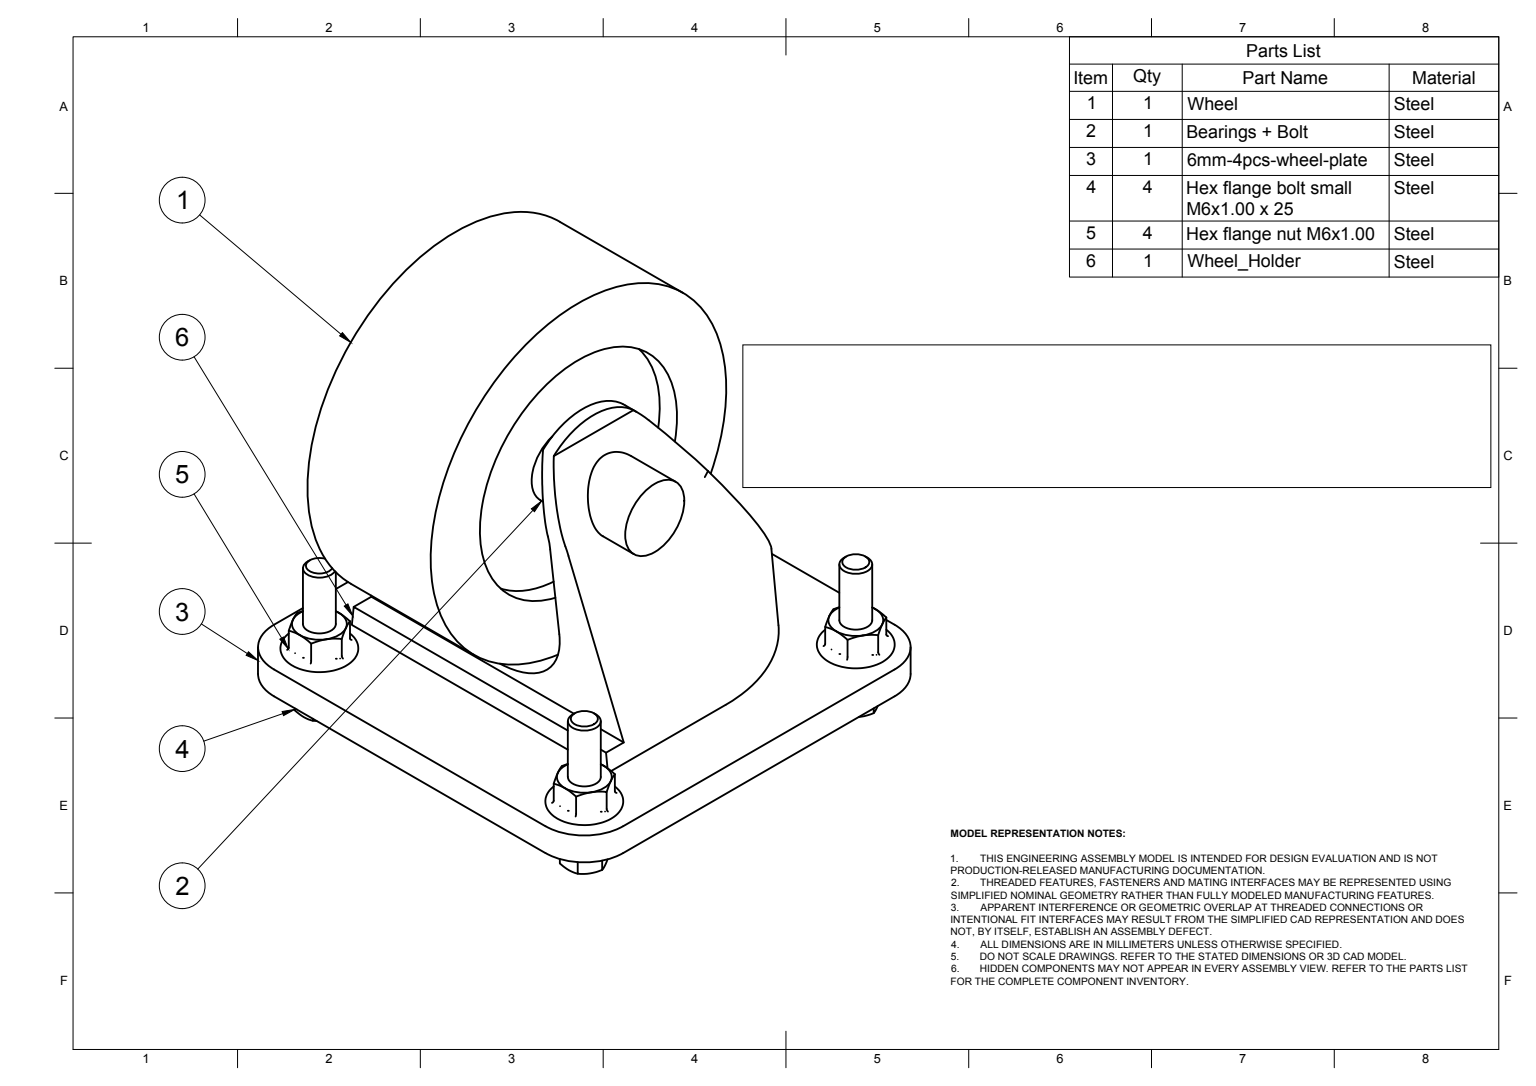
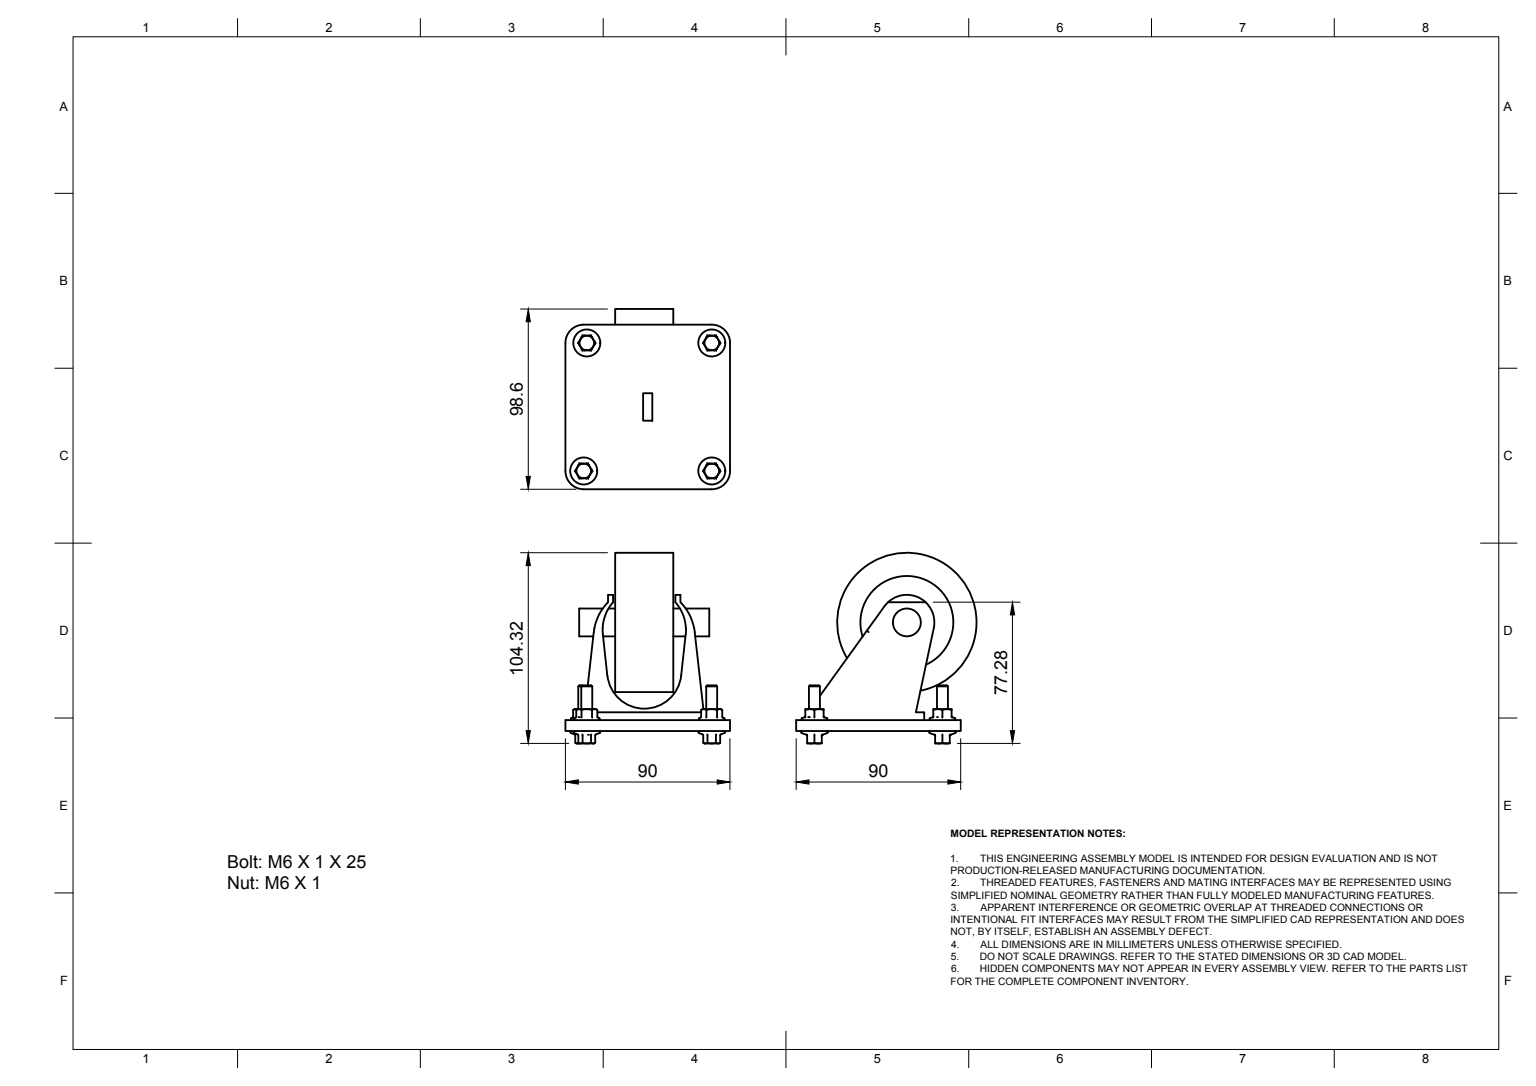
ISO-10303-21;
HEADER;
/* Generated by software containing ST-Developer
 * from STEP Tools, Inc. (www.steptools.com) 
 */

FILE_DESCRIPTION(
/* description */ ('Wheel Holder-Mirrored'),
/* implementation_level */ '2;1');

FILE_NAME(
/* name */ 'MAS-606',
/* time_stamp */ '2026-10-07T09:01:46-07:00',
/* author */ (''),
/* organization */ (''),
/* preprocessor_version */ 'ST-DEVELOPER v20.2',
/* originating_system */ 'Autodesk Translation Framework v15.15.0.0',
/* authorisation */ '');

FILE_SCHEMA (('AUTOMOTIVE_DESIGN { 1 0 10303 214 3 1 1 }'));
ENDSEC;

DATA;
#10=MECHANICAL_DESIGN_GEOMETRIC_PRESENTATION_REPRESENTATION('',(#198,#199,
#200,#201,#202,#203),#3832);
#11=ITEM_DEFINED_TRANSFORMATION($,$,#1857,#2036);
#12=ITEM_DEFINED_TRANSFORMATION($,$,#1874,#2037);
#13=ITEM_DEFINED_TRANSFORMATION($,$,#1880,#2038);
#14=ITEM_DEFINED_TRANSFORMATION($,$,#1915,#2039);
#15=ITEM_DEFINED_TRANSFORMATION($,$,#1951,#2040);
#16=ITEM_DEFINED_TRANSFORMATION($,$,#1915,#2041);
#17=ITEM_DEFINED_TRANSFORMATION($,$,#1915,#2042);
#18=ITEM_DEFINED_TRANSFORMATION($,$,#1915,#2043);
#19=ITEM_DEFINED_TRANSFORMATION($,$,#1951,#2044);
#20=ITEM_DEFINED_TRANSFORMATION($,$,#1951,#2045);
#21=ITEM_DEFINED_TRANSFORMATION($,$,#1951,#2046);
#22=ITEM_DEFINED_TRANSFORMATION($,$,#1986,#2047);
#23=(
REPRESENTATION_RELATIONSHIP($,$,#3863,#3862)
REPRESENTATION_RELATIONSHIP_WITH_TRANSFORMATION(#11)
SHAPE_REPRESENTATION_RELATIONSHIP()
);
#24=(
REPRESENTATION_RELATIONSHIP($,$,#3864,#3862)
REPRESENTATION_RELATIONSHIP_WITH_TRANSFORMATION(#12)
SHAPE_REPRESENTATION_RELATIONSHIP()
);
#25=(
REPRESENTATION_RELATIONSHIP($,$,#3865,#3862)
REPRESENTATION_RELATIONSHIP_WITH_TRANSFORMATION(#13)
SHAPE_REPRESENTATION_RELATIONSHIP()
);
#26=(
REPRESENTATION_RELATIONSHIP($,$,#3866,#3862)
REPRESENTATION_RELATIONSHIP_WITH_TRANSFORMATION(#14)
SHAPE_REPRESENTATION_RELATIONSHIP()
);
#27=(
REPRESENTATION_RELATIONSHIP($,$,#3867,#3862)
REPRESENTATION_RELATIONSHIP_WITH_TRANSFORMATION(#15)
SHAPE_REPRESENTATION_RELATIONSHIP()
);
#28=(
REPRESENTATION_RELATIONSHIP($,$,#3866,#3862)
REPRESENTATION_RELATIONSHIP_WITH_TRANSFORMATION(#16)
SHAPE_REPRESENTATION_RELATIONSHIP()
);
#29=(
REPRESENTATION_RELATIONSHIP($,$,#3866,#3862)
REPRESENTATION_RELATIONSHIP_WITH_TRANSFORMATION(#17)
SHAPE_REPRESENTATION_RELATIONSHIP()
);
#30=(
REPRESENTATION_RELATIONSHIP($,$,#3866,#3862)
REPRESENTATION_RELATIONSHIP_WITH_TRANSFORMATION(#18)
SHAPE_REPRESENTATION_RELATIONSHIP()
);
#31=(
REPRESENTATION_RELATIONSHIP($,$,#3867,#3862)
REPRESENTATION_RELATIONSHIP_WITH_TRANSFORMATION(#19)
SHAPE_REPRESENTATION_RELATIONSHIP()
);
#32=(
REPRESENTATION_RELATIONSHIP($,$,#3867,#3862)
REPRESENTATION_RELATIONSHIP_WITH_TRANSFORMATION(#20)
SHAPE_REPRESENTATION_RELATIONSHIP()
);
#33=(
REPRESENTATION_RELATIONSHIP($,$,#3867,#3862)
REPRESENTATION_RELATIONSHIP_WITH_TRANSFORMATION(#21)
SHAPE_REPRESENTATION_RELATIONSHIP()
);
#34=(
REPRESENTATION_RELATIONSHIP($,$,#3868,#3862)
REPRESENTATION_RELATIONSHIP_WITH_TRANSFORMATION(#22)
SHAPE_REPRESENTATION_RELATIONSHIP()
);
#35=CONTEXT_DEPENDENT_SHAPE_REPRESENTATION(#23,#3850);
#36=CONTEXT_DEPENDENT_SHAPE_REPRESENTATION(#24,#3851);
#37=CONTEXT_DEPENDENT_SHAPE_REPRESENTATION(#25,#3852);
#38=CONTEXT_DEPENDENT_SHAPE_REPRESENTATION(#26,#3853);
#39=CONTEXT_DEPENDENT_SHAPE_REPRESENTATION(#27,#3854);
#40=CONTEXT_DEPENDENT_SHAPE_REPRESENTATION(#28,#3855);
#41=CONTEXT_DEPENDENT_SHAPE_REPRESENTATION(#29,#3856);
#42=CONTEXT_DEPENDENT_SHAPE_REPRESENTATION(#30,#3857);
#43=CONTEXT_DEPENDENT_SHAPE_REPRESENTATION(#31,#3858);
#44=CONTEXT_DEPENDENT_SHAPE_REPRESENTATION(#32,#3859);
#45=CONTEXT_DEPENDENT_SHAPE_REPRESENTATION(#33,#3860);
#46=CONTEXT_DEPENDENT_SHAPE_REPRESENTATION(#34,#3861);
#47=NEXT_ASSEMBLY_USAGE_OCCURRENCE('Wheel:1','Wheel:1','Wheel:1',#3870,
#3871,'Wheel:1');
#48=NEXT_ASSEMBLY_USAGE_OCCURRENCE('Bearings + Bolt:1',
'Bearings + Bolt:1','Bearings + Bolt:1',#3870,#3872,'Bearings + Bolt:1');
#49=NEXT_ASSEMBLY_USAGE_OCCURRENCE('Wheel_Plate:1','Wheel_Plate:1',
'Wheel_Plate:1',#3870,#3873,'Wheel_Plate:1');
#50=NEXT_ASSEMBLY_USAGE_OCCURRENCE(
'Hex flange bolt small M6x1.00 x 25:1',
'Hex flange bolt small M6x1.00 x 25:1',
'Hex flange bolt small M6x1.00 x 25:1',#3870,#3874,
'Hex flange bolt small M6x1.00 x 25:1');
#51=NEXT_ASSEMBLY_USAGE_OCCURRENCE('Hex flange nut M6x1.00:1',
'Hex flange nut M6x1.00:1','Hex flange nut M6x1.00:1',#3870,#3875,
'Hex flange nut M6x1.00:1');
#52=NEXT_ASSEMBLY_USAGE_OCCURRENCE(
'Hex flange bolt small M6x1.00 x 25:2',
'Hex flange bolt small M6x1.00 x 25:2',
'Hex flange bolt small M6x1.00 x 25:2',#3870,#3874,
'Hex flange bolt small M6x1.00 x 25:2');
#53=NEXT_ASSEMBLY_USAGE_OCCURRENCE(
'Hex flange bolt small M6x1.00 x 25:3',
'Hex flange bolt small M6x1.00 x 25:3',
'Hex flange bolt small M6x1.00 x 25:3',#3870,#3874,
'Hex flange bolt small M6x1.00 x 25:3');
#54=NEXT_ASSEMBLY_USAGE_OCCURRENCE(
'Hex flange bolt small M6x1.00 x 25:4',
'Hex flange bolt small M6x1.00 x 25:4',
'Hex flange bolt small M6x1.00 x 25:4',#3870,#3874,
'Hex flange bolt small M6x1.00 x 25:4');
#55=NEXT_ASSEMBLY_USAGE_OCCURRENCE('Hex flange nut M6x1.00:2',
'Hex flange nut M6x1.00:2','Hex flange nut M6x1.00:2',#3870,#3875,
'Hex flange nut M6x1.00:2');
#56=NEXT_ASSEMBLY_USAGE_OCCURRENCE('Hex flange nut M6x1.00:3',
'Hex flange nut M6x1.00:3','Hex flange nut M6x1.00:3',#3870,#3875,
'Hex flange nut M6x1.00:3');
#57=NEXT_ASSEMBLY_USAGE_OCCURRENCE('Hex flange nut M6x1.00:4',
'Hex flange nut M6x1.00:4','Hex flange nut M6x1.00:4',#3870,#3875,
'Hex flange nut M6x1.00:4');
#58=NEXT_ASSEMBLY_USAGE_OCCURRENCE('Wheel_Holder:1','Wheel_Holder:1',
'Wheel_Holder:1',#3870,#3876,'Wheel_Holder:1');
#59=ELLIPSE('',#1988,0.00766814592499653,0.00762);
#60=ELLIPSE('',#1989,0.0076644002839305,0.00762);
#61=ELLIPSE('',#1993,0.0342294027026876,0.0277785949688766);
#62=ELLIPSE('',#1994,0.028399185304996,0.0277785949688766);
#63=ELLIPSE('',#2002,0.0232756976080203,0.0227670677706907);
#64=ELLIPSE('',#2003,0.0280540873991463,0.0227670677706907);
#65=ELLIPSE('',#2005,0.0232756976080203,0.0227670677706907);
#66=ELLIPSE('',#2006,0.0280540873991463,0.0227670677706907);
#67=ELLIPSE('',#2009,0.0207739608876574,0.02032);
#68=ELLIPSE('',#2010,0.0250387560529214,0.02032);
#69=ELLIPSE('',#2012,0.0076644002839305,0.00762);
#70=ELLIPSE('',#2016,0.0283991853049961,0.0277785949688767);
#71=ELLIPSE('',#2021,0.0570304735096183,0.0331133532215094);
#72=ELLIPSE('',#2022,0.0342294027026876,0.0277785949688767);
#73=ELLIPSE('',#2023,0.0570304735096183,0.0331133532215094);
#74=ELLIPSE('',#2025,0.0333225754026887,0.0331133532215094);
#75=ELLIPSE('',#2026,0.0333225754026887,0.0331133532215094);
#76=ELLIPSE('',#2028,0.00766814592499653,0.00762);
#77=ELLIPSE('',#2034,0.295962272640151,0.0331133532215094);
#78=(
BOUNDED_SURFACE()
B_SPLINE_SURFACE(3,2,((#2888,#2889,#2890),(#2891,#2892,#2893),(#2894,#2895,
#2896),(#2897,#2898,#2899),(#2900,#2901,#2902)),.UNSPECIFIED.,.F.,.F.,.F.)
B_SPLINE_SURFACE_WITH_KNOTS((4,1,4),(3,3),(0.0199905421078539,0.0227092821601536,
0.0254280222134474),(0.,1.00056005679341),.UNSPECIFIED.)
GEOMETRIC_REPRESENTATION_ITEM()
RATIONAL_B_SPLINE_SURFACE(((1.,0.802854637372621,1.00022082519925),(1.,
0.81108958019377,1.00021160112791),(1.,0.82690910145913,1.00019388146721),
(1.,0.811291833393597,1.00021137458136),(1.,0.802795753782992,1.00022089115557)))
REPRESENTATION_ITEM('')
SURFACE()
);
#79=(
BOUNDED_SURFACE()
B_SPLINE_SURFACE(3,2,((#2927,#2928,#2929),(#2930,#2931,#2932),(#2933,#2934,
#2935),(#2936,#2937,#2938),(#2939,#2940,#2941)),.UNSPECIFIED.,.F.,.F.,.F.)
B_SPLINE_SURFACE_WITH_KNOTS((4,1,4),(3,3),(0.0199863987269074,0.0227063701116868,
0.0254263415355543),(0.,1.00056355085534),.UNSPECIFIED.)
GEOMETRIC_REPRESENTATION_ITEM()
RATIONAL_B_SPLINE_SURFACE(((1.,0.802841957060873,1.00022221716746),(1.,
0.811080854660757,1.00021293109189),(1.,0.826916200792063,1.00019508304617),
(1.,0.811283787847418,1.00021270236556),(1.,0.802782519169589,1.00022228416001)))
REPRESENTATION_ITEM('')
SURFACE()
);
#80=(
BOUNDED_SURFACE()
B_SPLINE_SURFACE(3,2,((#2954,#2955,#2956),(#2957,#2958,#2959),(#2960,#2961,
#2962),(#2963,#2964,#2965),(#2966,#2967,#2968)),.UNSPECIFIED.,.F.,.F.,.F.)
B_SPLINE_SURFACE_WITH_KNOTS((4,1,4),(3,3),(0.0199905421079487,0.0227092821601536,
0.0254280222133526),(0.,1.00056005680003),.UNSPECIFIED.)
GEOMETRIC_REPRESENTATION_ITEM()
RATIONAL_B_SPLINE_SURFACE(((1.,0.802854637372034,1.00022082520187),(1.,
0.811089580193672,1.00021160113042),(1.,0.826909101456828,1.00019388146951),
(1.,0.81129183339351,1.00021137458386),(1.,0.802795753782428,1.00022089115817)))
REPRESENTATION_ITEM('')
SURFACE()
);
#81=(
BOUNDED_SURFACE()
B_SPLINE_SURFACE(3,2,((#2981,#2982,#2983),(#2984,#2985,#2986),(#2987,#2988,
#2989),(#2990,#2991,#2992),(#2993,#2994,#2995)),.UNSPECIFIED.,.F.,.F.,.F.)
B_SPLINE_SURFACE_WITH_KNOTS((4,1,4),(3,3),(0.0199905421080522,0.0227092821601536,
0.0254280222132491),(0.,1.00056005679973),.UNSPECIFIED.)
GEOMETRIC_REPRESENTATION_ITEM()
RATIONAL_B_SPLINE_SURFACE(((1.,0.802854637372995,1.00022082520174),(1.,
0.811089580194489,1.00021160113031),(1.,0.826909101456198,1.0001938814694),
(1.,0.811291833394166,1.00021137458374),(1.,0.802795753783457,1.00022089115806)))
REPRESENTATION_ITEM('')
SURFACE()
);
#82=(
BOUNDED_SURFACE()
B_SPLINE_SURFACE(3,2,((#3008,#3009,#3010),(#3011,#3012,#3013),(#3014,#3015,
#3016),(#3017,#3018,#3019),(#3020,#3021,#3022)),.UNSPECIFIED.,.F.,.F.,.F.)
B_SPLINE_SURFACE_WITH_KNOTS((4,1,4),(3,3),(0.019994704332767,0.022712204724463,
0.0254297050789377),(0.,1.00055654499458),.UNSPECIFIED.)
GEOMETRIC_REPRESENTATION_ITEM()
RATIONAL_B_SPLINE_SURFACE(((1.,0.802867397371381,1.00021942632651),(1.,
0.811098353635701,1.00021026453151),(1.,0.826901960236561,1.00019267369521),
(1.,0.811299927383003,1.00021004016178),(1.,0.802809067580306,1.00021949125283)))
REPRESENTATION_ITEM('')
SURFACE()
);
#83=(
BOUNDED_SURFACE()
B_SPLINE_SURFACE(3,2,((#3035,#3036,#3037),(#3038,#3039,#3040),(#3041,#3042,
#3043),(#3044,#3045,#3046),(#3047,#3048,#3049)),.UNSPECIFIED.,.F.,.F.,.F.)
B_SPLINE_SURFACE_WITH_KNOTS((4,1,4),(3,3),(0.0199905421078943,0.0227092821601536,
0.025428022213407),(0.,1.00056005680679),.UNSPECIFIED.)
GEOMETRIC_REPRESENTATION_ITEM()
RATIONAL_B_SPLINE_SURFACE(((1.,0.802854637370352,1.00022082520454),(1.,
0.811089580191479,1.00021160113298),(1.,0.826909101456581,1.00019388147184),
(1.,0.811291833391307,1.00021137458641),(1.,0.802795753780734,1.00022089116085)))
REPRESENTATION_ITEM('')
SURFACE()
);
#84=(
BOUNDED_SURFACE()
B_SPLINE_SURFACE(3,2,((#3298,#3299,#3300),(#3301,#3302,#3303),(#3304,#3305,
#3306),(#3307,#3308,#3309),(#3310,#3311,#3312)),.UNSPECIFIED.,.F.,.F.,.F.)
B_SPLINE_SURFACE_WITH_KNOTS((4,1,4),(3,3),(0.0246620904109836,0.0279939304185144,
0.0313257704892837),(0.,1.00067047018092),.UNSPECIFIED.)
GEOMETRIC_REPRESENTATION_ITEM()
RATIONAL_B_SPLINE_SURFACE(((1.,0.802865969663045,1.00026434497797),(1.,
0.81108910405605,1.00025331824517),(1.,0.82686917993846,1.0002321581045),
(1.,0.81129221048254,1.00025304589156),(1.,0.802807804958138,1.00026442297338)))
REPRESENTATION_ITEM('')
SURFACE()
);
#85=(
BOUNDED_SURFACE()
B_SPLINE_SURFACE(3,2,((#3337,#3338,#3339),(#3340,#3341,#3342),(#3343,#3344,
#3345),(#3346,#3347,#3348),(#3349,#3350,#3351)),.UNSPECIFIED.,.F.,.F.,.F.)
B_SPLINE_SURFACE_WITH_KNOTS((4,1,4),(3,3),(0.024738817097226,0.0280688166766824,
0.0313988162601249),(0.,1.00066549850917),.UNSPECIFIED.)
GEOMETRIC_REPRESENTATION_ITEM()
RATIONAL_B_SPLINE_SURFACE(((1.,0.802880827397706,1.00026236503099),(1.,
0.811099228845429,1.00025142636317),(1.,0.82686120340028,1.00023044722203),
(1.,0.811301685281914,1.00025115689426),(1.,0.80282325859447,1.0002624416549)))
REPRESENTATION_ITEM('')
SURFACE()
);
#86=(
BOUNDED_SURFACE()
B_SPLINE_SURFACE(3,2,((#3364,#3365,#3366),(#3367,#3368,#3369),(#3370,#3371,
#3372),(#3373,#3374,#3375),(#3376,#3377,#3378)),.UNSPECIFIED.,.F.,.F.,.F.)
B_SPLINE_SURFACE_WITH_KNOTS((4,1,4),(3,3),(0.024738817096804,0.0280688166766824,
0.0313988162605461),(0.,1.00066549851789),.UNSPECIFIED.)
GEOMETRIC_REPRESENTATION_ITEM()
RATIONAL_B_SPLINE_SURFACE(((1.,0.802880827392752,1.00026236503443),(1.,
0.811099228842278,1.00025142636647),(1.,0.826861203399938,1.00023044722505),
(1.,0.811301685279444,1.00025115689755),(1.,0.802823258589269,1.00026244165835)))
REPRESENTATION_ITEM('')
SURFACE()
);
#87=(
BOUNDED_SURFACE()
B_SPLINE_SURFACE(3,2,((#3391,#3392,#3393),(#3394,#3395,#3396),(#3397,#3398,
#3399),(#3400,#3401,#3402),(#3403,#3404,#3405)),.UNSPECIFIED.,.F.,.F.,.F.)
B_SPLINE_SURFACE_WITH_KNOTS((4,1,4),(3,3),(0.0247388170968889,0.0280688166766824,
0.0313988162604618),(0.,1.00066549851781),.UNSPECIFIED.)
GEOMETRIC_REPRESENTATION_ITEM()
RATIONAL_B_SPLINE_SURFACE(((1.,0.802880827393329,1.00026236503441),(1.,
0.811099228842959,1.00025142636643),(1.,0.82686120340021,1.00023044722503),
(1.,0.811301685278279,1.00025115689751),(1.,0.802823258590303,1.0002624416583)))
REPRESENTATION_ITEM('')
SURFACE()
);
#88=(
BOUNDED_SURFACE()
B_SPLINE_SURFACE(3,2,((#3418,#3419,#3420),(#3421,#3422,#3423),(#3424,#3425,
#3426),(#3427,#3428,#3429),(#3430,#3431,#3432)),.UNSPECIFIED.,.F.,.F.,.F.)
B_SPLINE_SURFACE_WITH_KNOTS((4,1,4),(3,3),(0.0247388170974279,0.0280688166766824,
0.031398816259923),(0.,1.00066549852508),.UNSPECIFIED.)
GEOMETRIC_REPRESENTATION_ITEM()
RATIONAL_B_SPLINE_SURFACE(((1.,0.802880827396021,1.00026236503726),(1.,
0.811099228843575,1.00025142636918),(1.,0.826861203396443,1.00023044722754),
(1.,0.811301685279931,1.00025115690027),(1.,0.80282325859286,1.00026244166118)))
REPRESENTATION_ITEM('')
SURFACE()
);
#89=(
BOUNDED_SURFACE()
B_SPLINE_SURFACE(3,2,((#3445,#3446,#3447),(#3448,#3449,#3450),(#3451,#3452,
#3453),(#3454,#3455,#3456),(#3457,#3458,#3459)),.UNSPECIFIED.,.F.,.F.,.F.)
B_SPLINE_SURFACE_WITH_KNOTS((4,1,4),(3,3),(0.0246749646102296,0.0280029916911416,
0.031331018716321),(0.,1.00065966906838),.UNSPECIFIED.)
GEOMETRIC_REPRESENTATION_ITEM()
RATIONAL_B_SPLINE_SURFACE(((1.,0.802898366215555,1.00026004370227),(1.,
0.811111461933951,1.00024920785186),(1.,0.826851645151749,1.00022844122787),
(1.,0.811312849119053,1.00024894215407),(1.,0.802841584394648,1.00026011861669)))
REPRESENTATION_ITEM('')
SURFACE()
);
#90=TOROIDAL_SURFACE('',#1935,0.0068,0.000567100162269167);
#91=TOROIDAL_SURFACE('',#1948,0.00325,0.00025);
#92=TOROIDAL_SURFACE('',#1982,0.00653289983773083,0.000567100162269171);
#93=CONICAL_SURFACE('',#1922,0.004,1.0471975511966);
#94=CONICAL_SURFACE('',#1924,0.004,1.0471975511966);
#95=CONICAL_SURFACE('',#1926,0.004,1.0471975511966);
#96=CONICAL_SURFACE('',#1928,0.004,1.0471975511966);
#97=CONICAL_SURFACE('',#1930,0.004,1.0471975511966);
#98=CONICAL_SURFACE('',#1932,0.004,1.0471975511966);
#99=CONICAL_SURFACE('',#1940,1.,1.22173047639603);
#100=CONICAL_SURFACE('',#1950,0.002458734125,0.78539816339745);
#101=CONICAL_SURFACE('',#1973,0.005,1.0471975511966);
#102=CONICAL_SURFACE('',#1974,0.005,1.0471975511966);
#103=CONICAL_SURFACE('',#1975,0.005,1.0471975511966);
#104=CONICAL_SURFACE('',#1976,0.005,1.0471975511966);
#105=CONICAL_SURFACE('',#1977,0.005,1.0471975511966);
#106=CONICAL_SURFACE('',#1978,0.005,1.0471975511966);
#107=CONICAL_SURFACE('',#1979,0.00672685951651014,1.22173047639603);
#108=CONICAL_SURFACE('',#1984,0.003,0.785398163397448);
#109=CONICAL_SURFACE('',#1985,0.0024585,0.785398163397448);
#110=(
BOUNDED_CURVE()
B_SPLINE_CURVE(2,(#2688,#2689,#2690),.UNSPECIFIED.,.F.,.F.)
B_SPLINE_CURVE_WITH_KNOTS((3,3),(0.899640233852609,1.41204223156836),
 .UNSPECIFIED.)
CURVE()
GEOMETRIC_REPRESENTATION_ITEM()
RATIONAL_B_SPLINE_CURVE((2.04103265936813,2.19890708499154,2.19890708499154))
REPRESENTATION_ITEM('')
);
#111=(
BOUNDED_CURVE()
B_SPLINE_CURVE(2,(#2691,#2692,#2693),.UNSPECIFIED.,.F.,.F.)
B_SPLINE_CURVE_WITH_KNOTS((3,3),(1.41204223156836,1.92444422930209),
 .UNSPECIFIED.)
CURVE()
GEOMETRIC_REPRESENTATION_ITEM()
RATIONAL_B_SPLINE_CURVE((2.19890708499154,2.19890708499154,2.04103265935705))
REPRESENTATION_ITEM('')
);
#112=(
BOUNDED_CURVE()
B_SPLINE_CURVE(2,(#2715,#2716,#2717),.UNSPECIFIED.,.F.,.F.)
B_SPLINE_CURVE_WITH_KNOTS((3,3),(0.899640233852608,1.41204223156835),
 .UNSPECIFIED.)
CURVE()
GEOMETRIC_REPRESENTATION_ITEM()
RATIONAL_B_SPLINE_CURVE((2.04103265936813,2.19890708499154,2.19890708499154))
REPRESENTATION_ITEM('')
);
#113=(
BOUNDED_CURVE()
B_SPLINE_CURVE(2,(#2718,#2719,#2720),.UNSPECIFIED.,.F.,.F.)
B_SPLINE_CURVE_WITH_KNOTS((3,3),(1.41204223156835,1.9244442293021),
 .UNSPECIFIED.)
CURVE()
GEOMETRIC_REPRESENTATION_ITEM()
RATIONAL_B_SPLINE_CURVE((2.19890708499154,2.19890708499154,2.04103265935704))
REPRESENTATION_ITEM('')
);
#114=(
BOUNDED_CURVE()
B_SPLINE_CURVE(2,(#2742,#2743,#2744),.UNSPECIFIED.,.F.,.F.)
B_SPLINE_CURVE_WITH_KNOTS((3,3),(-1.41204232189231,-0.899640300628516),
 .UNSPECIFIED.)
CURVE()
GEOMETRIC_REPRESENTATION_ITEM()
RATIONAL_B_SPLINE_CURVE((2.19890717995419,2.19890717995419,2.04103274751277))
REPRESENTATION_ITEM('')
);
#115=(
BOUNDED_CURVE()
B_SPLINE_CURVE(2,(#2745,#2746,#2747),.UNSPECIFIED.,.F.,.F.)
B_SPLINE_CURVE_WITH_KNOTS((3,3),(-1.9244443431741,-1.41204232189231),
 .UNSPECIFIED.)
CURVE()
GEOMETRIC_REPRESENTATION_ITEM()
RATIONAL_B_SPLINE_CURVE((2.04103274750169,2.19890717995419,2.19890717995419))
REPRESENTATION_ITEM('')
);
#116=(
BOUNDED_CURVE()
B_SPLINE_CURVE(2,(#2769,#2770,#2771),.UNSPECIFIED.,.F.,.F.)
B_SPLINE_CURVE_WITH_KNOTS((3,3),(0.899640233852631,1.41204223156839),
 .UNSPECIFIED.)
CURVE()
GEOMETRIC_REPRESENTATION_ITEM()
RATIONAL_B_SPLINE_CURVE((2.04103265936816,2.19890708499158,2.19890708499158))
REPRESENTATION_ITEM('')
);
#117=(
BOUNDED_CURVE()
B_SPLINE_CURVE(2,(#2772,#2773,#2774),.UNSPECIFIED.,.F.,.F.)
B_SPLINE_CURVE_WITH_KNOTS((3,3),(1.41204223156839,1.92444422930213),
 .UNSPECIFIED.)
CURVE()
GEOMETRIC_REPRESENTATION_ITEM()
RATIONAL_B_SPLINE_CURVE((2.19890708499158,2.19890708499158,2.04103265935708))
REPRESENTATION_ITEM('')
);
#118=(
BOUNDED_CURVE()
B_SPLINE_CURVE(2,(#2796,#2797,#2798),.UNSPECIFIED.,.F.,.F.)
B_SPLINE_CURVE_WITH_KNOTS((3,3),(0.899640233852618,1.41204223156836),
 .UNSPECIFIED.)
CURVE()
GEOMETRIC_REPRESENTATION_ITEM()
RATIONAL_B_SPLINE_CURVE((2.04103265936815,2.19890708499156,2.19890708499156))
REPRESENTATION_ITEM('')
);
#119=(
BOUNDED_CURVE()
B_SPLINE_CURVE(2,(#2799,#2800,#2801),.UNSPECIFIED.,.F.,.F.)
B_SPLINE_CURVE_WITH_KNOTS((3,3),(1.41204223156836,1.92444422930211),
 .UNSPECIFIED.)
CURVE()
GEOMETRIC_REPRESENTATION_ITEM()
RATIONAL_B_SPLINE_CURVE((2.19890708499156,2.19890708499156,2.04103265935706))
REPRESENTATION_ITEM('')
);
#120=(
BOUNDED_CURVE()
B_SPLINE_CURVE(2,(#2820,#2821,#2822),.UNSPECIFIED.,.F.,.F.)
B_SPLINE_CURVE_WITH_KNOTS((3,3),(0.899640166945249,1.4120421410666),
 .UNSPECIFIED.)
CURVE()
GEOMETRIC_REPRESENTATION_ITEM()
RATIONAL_B_SPLINE_CURVE((2.04103257104998,2.19890698984196,2.19890698984195))
REPRESENTATION_ITEM('')
);
#121=(
BOUNDED_CURVE()
B_SPLINE_CURVE(2,(#2823,#2824,#2825),.UNSPECIFIED.,.F.,.F.)
B_SPLINE_CURVE_WITH_KNOTS((3,3),(1.4120421410666,1.92444411520593),
 .UNSPECIFIED.)
CURVE()
GEOMETRIC_REPRESENTATION_ITEM()
RATIONAL_B_SPLINE_CURVE((2.19890698984195,2.19890698984195,2.04103257103889))
REPRESENTATION_ITEM('')
);
#122=(
BOUNDED_CURVE()
B_SPLINE_CURVE(2,(#3088,#3089,#3090),.UNSPECIFIED.,.F.,.F.)
B_SPLINE_CURVE_WITH_KNOTS((3,3),(0.868406024324111,1.41937586994552),
 .UNSPECIFIED.)
CURVE()
GEOMETRIC_REPRESENTATION_ITEM()
RATIONAL_B_SPLINE_CURVE((1.77300211797113,1.91014430907105,1.91014430907105))
REPRESENTATION_ITEM('')
);
#123=(
BOUNDED_CURVE()
B_SPLINE_CURVE(2,(#3091,#3092,#3093),.UNSPECIFIED.,.F.,.F.)
B_SPLINE_CURVE_WITH_KNOTS((3,3),(1.41937586994552,1.97034571556692),
 .UNSPECIFIED.)
CURVE()
GEOMETRIC_REPRESENTATION_ITEM()
RATIONAL_B_SPLINE_CURVE((1.91014430907105,1.91014430907105,1.77300211797113))
REPRESENTATION_ITEM('')
);
#124=(
BOUNDED_CURVE()
B_SPLINE_CURVE(2,(#3115,#3116,#3117),.UNSPECIFIED.,.F.,.F.)
B_SPLINE_CURVE_WITH_KNOTS((3,3),(0.868406111432395,1.41937598717132),
 .UNSPECIFIED.)
CURVE()
GEOMETRIC_REPRESENTATION_ITEM()
RATIONAL_B_SPLINE_CURVE((1.7730022081019,1.91014440617345,1.91014440617345))
REPRESENTATION_ITEM('')
);
#125=(
BOUNDED_CURVE()
B_SPLINE_CURVE(2,(#3118,#3119,#3120),.UNSPECIFIED.,.F.,.F.)
B_SPLINE_CURVE_WITH_KNOTS((3,3),(1.41937598717132,1.97034586291024),
 .UNSPECIFIED.)
CURVE()
GEOMETRIC_REPRESENTATION_ITEM()
RATIONAL_B_SPLINE_CURVE((1.91014440617345,1.91014440617345,1.7730022081019))
REPRESENTATION_ITEM('')
);
#126=(
BOUNDED_CURVE()
B_SPLINE_CURVE(2,(#3142,#3143,#3144),.UNSPECIFIED.,.F.,.F.)
B_SPLINE_CURVE_WITH_KNOTS((3,3),(0.868406111432417,1.41937598717135),
 .UNSPECIFIED.)
CURVE()
GEOMETRIC_REPRESENTATION_ITEM()
RATIONAL_B_SPLINE_CURVE((1.77300220810192,1.91014440617348,1.91014440617348))
REPRESENTATION_ITEM('')
);
#127=(
BOUNDED_CURVE()
B_SPLINE_CURVE(2,(#3145,#3146,#3147),.UNSPECIFIED.,.F.,.F.)
B_SPLINE_CURVE_WITH_KNOTS((3,3),(1.41937598717135,1.97034586291028),
 .UNSPECIFIED.)
CURVE()
GEOMETRIC_REPRESENTATION_ITEM()
RATIONAL_B_SPLINE_CURVE((1.91014440617348,1.91014440617348,1.77300220810192))
REPRESENTATION_ITEM('')
);
#128=(
BOUNDED_CURVE()
B_SPLINE_CURVE(2,(#3169,#3170,#3171),.UNSPECIFIED.,.F.,.F.)
B_SPLINE_CURVE_WITH_KNOTS((3,3),(-1.41937608879025,-0.868406186943507),
 .UNSPECIFIED.)
CURVE()
GEOMETRIC_REPRESENTATION_ITEM()
RATIONAL_B_SPLINE_CURVE((1.91014449034812,1.91014449034812,1.7730022862331))
REPRESENTATION_ITEM('')
);
#129=(
BOUNDED_CURVE()
B_SPLINE_CURVE(2,(#3172,#3173,#3174),.UNSPECIFIED.,.F.,.F.)
B_SPLINE_CURVE_WITH_KNOTS((3,3),(-1.97034599063699,-1.41937608879025),
 .UNSPECIFIED.)
CURVE()
GEOMETRIC_REPRESENTATION_ITEM()
RATIONAL_B_SPLINE_CURVE((1.7730022862331,1.91014449034812,1.91014449034812))
REPRESENTATION_ITEM('')
);
#130=(
BOUNDED_CURVE()
B_SPLINE_CURVE(2,(#3196,#3197,#3198),.UNSPECIFIED.,.F.,.F.)
B_SPLINE_CURVE_WITH_KNOTS((3,3),(0.868406111432395,1.41937598717132),
 .UNSPECIFIED.)
CURVE()
GEOMETRIC_REPRESENTATION_ITEM()
RATIONAL_B_SPLINE_CURVE((1.7730022081019,1.91014440617345,1.91014440617345))
REPRESENTATION_ITEM('')
);
#131=(
BOUNDED_CURVE()
B_SPLINE_CURVE(2,(#3199,#3200,#3201),.UNSPECIFIED.,.F.,.F.)
B_SPLINE_CURVE_WITH_KNOTS((3,3),(1.41937598717132,1.97034586291024),
 .UNSPECIFIED.)
CURVE()
GEOMETRIC_REPRESENTATION_ITEM()
RATIONAL_B_SPLINE_CURVE((1.91014440617345,1.91014440617345,1.7730022081019))
REPRESENTATION_ITEM('')
);
#132=(
BOUNDED_CURVE()
B_SPLINE_CURVE(2,(#3220,#3221,#3222),.UNSPECIFIED.,.F.,.F.)
B_SPLINE_CURVE_WITH_KNOTS((3,3),(0.868406111432386,1.41937598717131),
 .UNSPECIFIED.)
CURVE()
GEOMETRIC_REPRESENTATION_ITEM()
RATIONAL_B_SPLINE_CURVE((1.77300220810189,1.91014440617345,1.91014440617345))
REPRESENTATION_ITEM('')
);
#133=(
BOUNDED_CURVE()
B_SPLINE_CURVE(2,(#3223,#3224,#3225),.UNSPECIFIED.,.F.,.F.)
B_SPLINE_CURVE_WITH_KNOTS((3,3),(1.41937598717131,1.97034586291023),
 .UNSPECIFIED.)
CURVE()
GEOMETRIC_REPRESENTATION_ITEM()
RATIONAL_B_SPLINE_CURVE((1.91014440617345,1.91014440617345,1.77300220810189))
REPRESENTATION_ITEM('')
);
#134=B_SPLINE_CURVE_WITH_KNOTS('',3,(#2669,#2670,#2671,#2672,#2673,#2674,
#2675,#2676,#2677,#2678,#2679,#2680,#2681,#2682,#2683,#2684),
 .UNSPECIFIED.,.F.,.F.,(4,3,3,3,3,4),(0.,0.00115933810312788,0.0023008628112466,
0.00231867620625576,0.00347801430938363,0.00463735241251151),
 .UNSPECIFIED.);
#135=B_SPLINE_CURVE_WITH_KNOTS('',3,(#2696,#2697,#2698,#2699,#2700,#2701,
#2702,#2703,#2704,#2705,#2706,#2707,#2708,#2709,#2710,#2711),
 .UNSPECIFIED.,.F.,.F.,(4,3,3,3,3,4),(1.55309542619116E-19,0.00115933810312788,
0.0023008628112466,0.00231867620625576,0.00347801430938364,0.00463735241251152),
 .UNSPECIFIED.);
#136=B_SPLINE_CURVE_WITH_KNOTS('',3,(#2723,#2724,#2725,#2726,#2727,#2728,
#2729,#2730,#2731,#2732,#2733,#2734,#2735,#2736,#2737,#2738),
 .UNSPECIFIED.,.F.,.F.,(4,3,3,3,3,4),(0.,0.00115932447661246,0.00230074676248248,
0.00231864895322491,0.00347797342983737,0.00463729790644982),
 .UNSPECIFIED.);
#137=B_SPLINE_CURVE_WITH_KNOTS('',3,(#2750,#2751,#2752,#2753,#2754,#2755,
#2756,#2757,#2758,#2759,#2760,#2761,#2762,#2763,#2764,#2765),
 .UNSPECIFIED.,.F.,.F.,(4,3,3,3,3,4),(0.,0.00115933810312788,0.0023008628112466,
0.00231867620625576,0.00347801430938363,0.00463735241251151),
 .UNSPECIFIED.);
#138=B_SPLINE_CURVE_WITH_KNOTS('',3,(#2777,#2778,#2779,#2780,#2781,#2782,
#2783,#2784,#2785,#2786,#2787,#2788,#2789,#2790,#2791,#2792),
 .UNSPECIFIED.,.F.,.F.,(4,3,3,3,3,4),(3.24894099173316E-19,0.00115933810312788,
0.0023008628112466,0.00231867620625576,0.00347801430938364,0.00463735241251152),
 .UNSPECIFIED.);
#139=B_SPLINE_CURVE_WITH_KNOTS('',3,(#2803,#2804,#2805,#2806,#2807,#2808,
#2809,#2810,#2811,#2812,#2813,#2814,#2815,#2816,#2817,#2818),
 .UNSPECIFIED.,.F.,.F.,(4,3,3,3,3,4),(0.,0.00115935174734299,0.00230097898664969,
0.00231870349468598,0.00347805524202897,0.00463740698937197),
 .UNSPECIFIED.);
#140=B_SPLINE_CURVE_WITH_KNOTS('',3,(#2851,#2852,#2853,#2854,#2855),
 .UNSPECIFIED.,.F.,.F.,(4,1,4),(0.,0.00248123639135078,0.00496246810726153),
 .UNSPECIFIED.);
#141=B_SPLINE_CURVE_WITH_KNOTS('',3,(#2857,#2858,#2859,#2860,#2861),
 .UNSPECIFIED.,.F.,.F.,(4,1,4),(0.,0.00248125883902994,0.00496251282372695),
 .UNSPECIFIED.);
#142=B_SPLINE_CURVE_WITH_KNOTS('',3,(#2863,#2864,#2865,#2866,#2867),
 .UNSPECIFIED.,.F.,.F.,(4,1,4),(0.,0.00248123639135078,0.00496246796815217),
 .UNSPECIFIED.);
#143=B_SPLINE_CURVE_WITH_KNOTS('',3,(#2869,#2870,#2871,#2872,#2873),
 .UNSPECIFIED.,.F.,.F.,(4,1,4),(0.,0.00248123639135079,0.00496246818443855),
 .UNSPECIFIED.);
#144=B_SPLINE_CURVE_WITH_KNOTS('',3,(#2875,#2876,#2877,#2878,#2879),
 .UNSPECIFIED.,.F.,.F.,(4,1,4),(0.,0.00248121396259867,0.00496242332668108),
 .UNSPECIFIED.);
#145=B_SPLINE_CURVE_WITH_KNOTS('',3,(#2880,#2881,#2882,#2883,#2884),
 .UNSPECIFIED.,.F.,.F.,(4,1,4),(0.,0.00248123639135079,0.00496246828961979),
 .UNSPECIFIED.);
#146=B_SPLINE_CURVE_WITH_KNOTS('',3,(#2903,#2904,#2905,#2906,#2907,#2908,
#2909,#2910,#2911,#2912,#2913,#2914),.UNSPECIFIED.,.F.,.F.,(4,2,2,2,2,4),
(-0.0536945210860223,-0.0408448591087579,-0.026670772721852,-0.0132475634127344,
0.,0.00261482960537117),.UNSPECIFIED.);
#147=B_SPLINE_CURVE_WITH_KNOTS('',3,(#2915,#2916,#2917,#2918,#2919,#2920,
#2921,#2922,#2923,#2924,#2925,#2926),.UNSPECIFIED.,.F.,.F.,(4,2,2,2,2,4),
(-0.0536943501278373,-0.0408447644220054,-0.0266707574515382,-0.0132475635493419,
0.,0.0026147568848072),.UNSPECIFIED.);
#148=B_SPLINE_CURVE_WITH_KNOTS('',3,(#2942,#2943,#2944,#2945,#2946,#2947,
#2948,#2949,#2950,#2951,#2952,#2953),.UNSPECIFIED.,.F.,.F.,(4,2,2,2,2,4),
(0.,0.0128045620123767,0.0269286898692442,0.0403044328139677,0.0535040873424465,
0.0561132593100496),.UNSPECIFIED.);
#149=B_SPLINE_CURVE_WITH_KNOTS('',3,(#2969,#2970,#2971,#2972,#2973,#2974,
#2975,#2976,#2977,#2978,#2979,#2980),.UNSPECIFIED.,.F.,.F.,(4,2,2,2,2,4),
(-0.0536946737885314,-0.0408450041369318,-0.0266709101282734,-0.0132476284737636,
0.,0.00261482249258708),.UNSPECIFIED.);
#150=B_SPLINE_CURVE_WITH_KNOTS('',3,(#2996,#2997,#2998,#2999,#3000,#3001,
#3002,#3003,#3004,#3005,#3006,#3007),.UNSPECIFIED.,.F.,.F.,(4,2,2,2,2,4),
(0.,0.0128045651857744,0.0269286883548746,0.0403044491788003,0.0535041176088484,
0.0561132658579917),.UNSPECIFIED.);
#151=B_SPLINE_CURVE_WITH_KNOTS('',3,(#3023,#3024,#3025,#3026,#3027,#3028,
#3029,#3030,#3031,#3032,#3033,#3034),.UNSPECIFIED.,.F.,.F.,(4,2,2,2,2,4),
(0.,0.012804574182279,0.0269287091649782,0.0403044718863404,0.0535041388980146,
0.0561134038245879),.UNSPECIFIED.);
#152=B_SPLINE_CURVE_WITH_KNOTS('',3,(#3069,#3070,#3071,#3072,#3073,#3074,
#3075,#3076,#3077,#3078,#3079,#3080,#3081,#3082,#3083,#3084),
 .UNSPECIFIED.,.F.,.F.,(4,3,3,3,3,4),(0.,0.00144938529899606,0.00287700433635734,
0.00289877059799213,0.00434815589698819,0.00579754119598426),
 .UNSPECIFIED.);
#153=B_SPLINE_CURVE_WITH_KNOTS('',3,(#3096,#3097,#3098,#3099,#3100,#3101,
#3102,#3103,#3104,#3105,#3106,#3107,#3108,#3109,#3110,#3111),
 .UNSPECIFIED.,.F.,.F.,(4,3,3,3,3,4),(0.,0.0014493633079017,0.00287680164649716,
0.0028987266158034,0.0043480899237051,0.0057974532316068),.UNSPECIFIED.);
#154=B_SPLINE_CURVE_WITH_KNOTS('',3,(#3123,#3124,#3125,#3126,#3127,#3128,
#3129,#3130,#3131,#3132,#3133,#3134,#3135,#3136,#3137,#3138),
 .UNSPECIFIED.,.F.,.F.,(4,3,3,3,3,4),(1.17946057326806E-18,0.0014493633079017,
0.00287680164649714,0.0028987266158034,0.0043480899237051,0.0057974532316068),
 .UNSPECIFIED.);
#155=B_SPLINE_CURVE_WITH_KNOTS('',3,(#3150,#3151,#3152,#3153,#3154,#3155,
#3156,#3157,#3158,#3159,#3160,#3161,#3162,#3163,#3164,#3165),
 .UNSPECIFIED.,.F.,.F.,(4,3,3,3,3,4),(0.,0.00144934135226602,0.00287664328376737,
0.00289868270453203,0.00434802405679805,0.00579736540906406),
 .UNSPECIFIED.);
#156=B_SPLINE_CURVE_WITH_KNOTS('',3,(#3177,#3178,#3179,#3180,#3181,#3182,
#3183,#3184,#3185,#3186,#3187,#3188,#3189,#3190,#3191,#3192),
 .UNSPECIFIED.,.F.,.F.,(4,3,3,3,3,4),(0.,0.0014493633079017,0.00287680164649716,
0.0028987266158034,0.0043480899237051,0.0057974532316068),.UNSPECIFIED.);
#157=B_SPLINE_CURVE_WITH_KNOTS('',3,(#3203,#3204,#3205,#3206,#3207,#3208,
#3209,#3210,#3211,#3212,#3213,#3214,#3215,#3216,#3217,#3218),
 .UNSPECIFIED.,.F.,.F.,(4,3,3,3,3,4),(3.71652746642586E-20,0.0014493633079017,
0.00287680164649716,0.0028987266158034,0.0043480899237051,0.0057974532316068),
 .UNSPECIFIED.);
#158=B_SPLINE_CURVE_WITH_KNOTS('',3,(#3261,#3262,#3263,#3264,#3265),
 .UNSPECIFIED.,.F.,.F.,(4,1,4),(0.,0.00306035141916462,0.00612069810971412),
 .UNSPECIFIED.);
#159=B_SPLINE_CURVE_WITH_KNOTS('',3,(#3267,#3268,#3269,#3270,#3271),
 .UNSPECIFIED.,.F.,.F.,(4,1,4),(0.,0.00306038411039262,0.00612076331150472),
 .UNSPECIFIED.);
#160=B_SPLINE_CURVE_WITH_KNOTS('',3,(#3273,#3274,#3275,#3276,#3277),
 .UNSPECIFIED.,.F.,.F.,(4,1,4),(0.,0.00306035141916462,0.00612069797754228),
 .UNSPECIFIED.);
#161=B_SPLINE_CURVE_WITH_KNOTS('',3,(#3279,#3280,#3281,#3282,#3283),
 .UNSPECIFIED.,.F.,.F.,(4,1,4),(0.,0.00306035141916462,0.0061206980316515),
 .UNSPECIFIED.);
#162=B_SPLINE_CURVE_WITH_KNOTS('',3,(#3285,#3286,#3287,#3288,#3289),
 .UNSPECIFIED.,.F.,.F.,(4,1,4),(0.,0.00306031874524394,0.00612063285858316),
 .UNSPECIFIED.);
#163=B_SPLINE_CURVE_WITH_KNOTS('',3,(#3290,#3291,#3292,#3293,#3294),
 .UNSPECIFIED.,.F.,.F.,(4,1,4),(0.,0.00306035141916462,0.0061206982998644),
 .UNSPECIFIED.);
#164=B_SPLINE_CURVE_WITH_KNOTS('',3,(#3313,#3314,#3315,#3316,#3317,#3318,
#3319,#3320,#3321,#3322,#3323,#3324),.UNSPECIFIED.,.F.,.F.,(4,2,2,2,2,4),
(0.,0.0128141897701953,0.02694790056044,0.0403327677820611,0.0535291831368547,
0.0561361462772446),.UNSPECIFIED.);
#165=B_SPLINE_CURVE_WITH_KNOTS('',3,(#3325,#3326,#3327,#3328,#3329,#3330,
#3331,#3332,#3333,#3334,#3335,#3336),.UNSPECIFIED.,.F.,.F.,(4,2,2,2,2,4),
(-0.0537148048665765,-0.0408567535476394,-0.0266745253232854,-0.0132433858241141,
0.,0.00261137592542538),.UNSPECIFIED.);
#166=B_SPLINE_CURVE_WITH_KNOTS('',3,(#3352,#3353,#3354,#3355,#3356,#3357,
#3358,#3359,#3360,#3361,#3362,#3363),.UNSPECIFIED.,.F.,.F.,(4,2,2,2,2,4),
(-0.0537150980019462,-0.040856939694021,-0.0266745961838983,-0.0132434100107398,
0.,0.00261147527362479),.UNSPECIFIED.);
#167=B_SPLINE_CURVE_WITH_KNOTS('',3,(#3379,#3380,#3381,#3382,#3383,#3384,
#3385,#3386,#3387,#3388,#3389,#3390),.UNSPECIFIED.,.F.,.F.,(4,2,2,2,2,4),
(0.,0.0128141921500334,0.0269478992409766,0.0403327871050577,0.0535292168707035,
0.0561361567166107),.UNSPECIFIED.);
#168=B_SPLINE_CURVE_WITH_KNOTS('',3,(#3406,#3407,#3408,#3409,#3410,#3411,
#3412,#3413,#3414,#3415,#3416,#3417),.UNSPECIFIED.,.F.,.F.,(4,2,2,2,2,4),
(-0.0537154001549951,-0.0408571973817338,-0.0266748056367786,-0.013243506422928,
0.,0.00261149488798623),.UNSPECIFIED.);
#169=B_SPLINE_CURVE_WITH_KNOTS('',3,(#3433,#3434,#3435,#3436,#3437,#3438,
#3439,#3440,#3441,#3442,#3443,#3444),.UNSPECIFIED.,.F.,.F.,(4,2,2,2,2,4),
(0.,0.0128142026815068,0.0269479237273733,0.0403328127900412,0.0535292370600361,
0.0561362028969855),.UNSPECIFIED.);
#170=B_SPLINE_CURVE_WITH_KNOTS('',3,(#3468,#3469,#3470,#3471,#3472,#3473,
#3474,#3475,#3476,#3477,#3478,#3479,#3480,#3481),.UNSPECIFIED.,.F.,.F.,
(4,2,2,2,2,2,4),(0.58453144748271,0.867768183831352,1.16094035782968,1.4691070433662,
1.77727372890272,2.07579244535874,2.37431116181475),.UNSPECIFIED.);
#171=B_SPLINE_CURVE_WITH_KNOTS('',3,(#3484,#3485,#3486,#3487,#3488,#3489,
#3490,#3491,#3492,#3493,#3494,#3495,#3496,#3497),.UNSPECIFIED.,.F.,.F.,
(4,2,2,2,2,2,4),(2.37431116181475,2.66483368462927,2.95535620744379,3.27144000918075,
3.58752381091772,3.88103472550587,4.16394043172282),.UNSPECIFIED.);
#172=B_SPLINE_CURVE_WITH_KNOTS('',3,(#3501,#3502,#3503,#3504,#3505,#3506,
#3507,#3508,#3509,#3510,#3511,#3512,#3513,#3514,#3515,#3516),
 .UNSPECIFIED.,.F.,.F.,(4,2,2,2,2,2,2,4),(-4.27790233879451,-4.09945168810992,
-3.81195458017329,-3.52445747223665,-3.22219845470822,-2.91993943717978,
-2.62905677671056,-2.33817411624134),.UNSPECIFIED.);
#173=B_SPLINE_CURVE_WITH_KNOTS('',3,(#3519,#3520,#3521,#3522,#3523,#3524,
#3525,#3526,#3527,#3528,#3529,#3530,#3531,#3532,#3533,#3534),
 .UNSPECIFIED.,.F.,.F.,(4,2,2,2,2,2,2,4),(-2.33817411624134,-2.04729145577211,
-1.75640879530289,-1.45414977777445,-1.15189076024602,-0.864393652309382,
-0.576896544372747,-0.398445893688138),.UNSPECIFIED.);
#174=B_SPLINE_CURVE_WITH_KNOTS('',3,(#3544,#3545,#3546,#3547,#3548,#3549,
#3550),.UNSPECIFIED.,.F.,.F.,(4,3,4),(-3.65201569549685,-3.58349548702897,
-3.30021421468191),.UNSPECIFIED.);
#175=B_SPLINE_CURVE_WITH_KNOTS('',3,(#3552,#3553,#3554,#3555,#3556,#3557,
#3558,#3559,#3560,#3561,#3562,#3563,#3564,#3565),.UNSPECIFIED.,.F.,.F.,
(4,2,2,2,2,2,4),(-7.77993041753592,-7.7480845912713,-7.46235224345222,-7.12519900195174,
-6.78804576045127,-6.11373927745031,-6.10347024465041),.UNSPECIFIED.);
#176=B_SPLINE_CURVE_WITH_KNOTS('',3,(#3596,#3597,#3598,#3599,#3600,#3601,
#3602,#3603,#3604,#3605,#3606,#3607,#3608,#3609),.UNSPECIFIED.,.F.,.F.,
(4,2,2,2,2,2,4),(-7.66118685225602,-7.63498959168202,-7.35041272704815,
-7.0310473742494,-6.71168202145065,-6.07295131585314,-6.03832591549393),
 .UNSPECIFIED.);
#177=B_SPLINE_CURVE_WITH_KNOTS('',3,(#3611,#3612,#3613,#3614,#3615,#3616),
 .UNSPECIFIED.,.F.,.F.,(4,2,4),(-3.62027438097633,-3.58564898061712,-3.28085403484185),
 .UNSPECIFIED.);
#178=B_SPLINE_CURVE_WITH_KNOTS('',3,(#3628,#3629,#3630,#3631,#3632,#3633,
#3634,#3635,#3636,#3637,#3638,#3639,#3640,#3641,#3642,#3643),
 .UNSPECIFIED.,.F.,.F.,(4,2,2,2,2,2,2,4),(0.398445893688145,0.576896544372747,
0.864393652309382,1.15189076024602,1.45414977777445,1.75640879530289,2.04729145577211,
2.33817411624133),.UNSPECIFIED.);
#179=B_SPLINE_CURVE_WITH_KNOTS('',3,(#3645,#3646,#3647,#3648,#3649,#3650,
#3651,#3652,#3653,#3654,#3655,#3656,#3657,#3658,#3659,#3660),
 .UNSPECIFIED.,.F.,.F.,(4,2,2,2,2,2,2,4),(2.33817411624133,2.62905677671056,
2.91993943717978,3.22219845470822,3.52445747223665,3.81195458017329,4.09945168810992,
4.27790233879452),.UNSPECIFIED.);
#180=B_SPLINE_CURVE_WITH_KNOTS('',3,(#3665,#3666,#3667,#3668,#3669,#3670),
 .UNSPECIFIED.,.F.,.F.,(4,2,4),(-6.38055499661601,-6.10670626645482,-6.04021537866389),
 .UNSPECIFIED.);
#181=B_SPLINE_CURVE_WITH_KNOTS('',3,(#3671,#3672,#3673,#3674,#3675,#3676,
#3677,#3678,#3679,#3680,#3681,#3682,#3683,#3684),.UNSPECIFIED.,.F.,.F.,
(4,2,2,2,2,2,4),(-3.62027438097633,-3.58564898061712,-2.94691827501961,
-2.62755292222086,-2.30818756942211,-2.02361070478824,-1.99741344421424),
 .UNSPECIFIED.);
#182=B_SPLINE_CURVE_WITH_KNOTS('',3,(#3724,#3725,#3726,#3727,#3728,#3729,
#3730),.UNSPECIFIED.,.F.,.F.,(4,3,4),(3.30021421468192,3.58349548702897,
3.65201569549685),.UNSPECIFIED.);
#183=B_SPLINE_CURVE_WITH_KNOTS('',3,(#3733,#3734,#3735,#3736,#3737,#3738,
#3739,#3740,#3741,#3742,#3743,#3744,#3745,#3746),.UNSPECIFIED.,.F.,.F.,
(4,2,2,2,2,2,4),(6.10060038618841,6.11086941898832,6.78517590198927,7.12232914348975,
7.45948238499022,7.7452147328093,7.77706055907392),.UNSPECIFIED.);
#184=B_SPLINE_CURVE_WITH_KNOTS('',3,(#3763,#3764,#3765,#3766,#3767,#3768,
#3769,#3770,#3771,#3772,#3773,#3774,#3775,#3776),.UNSPECIFIED.,.F.,.F.,
(4,2,2,2,2,2,4),(0.584524822753337,0.867430528970284,1.16094144355843,1.4770252452954,
1.79310904703237,2.08363156984688,2.3741540926614),.UNSPECIFIED.);
#185=B_SPLINE_CURVE_WITH_KNOTS('',3,(#3779,#3780,#3781,#3782,#3783,#3784,
#3785,#3786,#3787,#3788,#3789,#3790,#3791,#3792),.UNSPECIFIED.,.F.,.F.,
(4,2,2,2,2,2,4),(2.3741540926614,2.66467661547592,2.95519913829043,3.2712829400274,
3.58736674176437,3.88087765635252,4.16378336256947),.UNSPECIFIED.);
#186=SHAPE_REPRESENTATION_RELATIONSHIP('SRR','None',#3863,#192);
#187=SHAPE_REPRESENTATION_RELATIONSHIP('SRR','None',#3864,#193);
#188=SHAPE_REPRESENTATION_RELATIONSHIP('SRR','None',#3865,#194);
#189=SHAPE_REPRESENTATION_RELATIONSHIP('SRR','None',#3866,#195);
#190=SHAPE_REPRESENTATION_RELATIONSHIP('SRR','None',#3867,#196);
#191=SHAPE_REPRESENTATION_RELATIONSHIP('SRR','None',#3868,#197);
#192=ADVANCED_BREP_SHAPE_REPRESENTATION('',(#204),#3826);
#193=ADVANCED_BREP_SHAPE_REPRESENTATION('',(#205),#3827);
#194=ADVANCED_BREP_SHAPE_REPRESENTATION('',(#206),#3828);
#195=ADVANCED_BREP_SHAPE_REPRESENTATION('',(#207),#3829);
#196=ADVANCED_BREP_SHAPE_REPRESENTATION('',(#208),#3830);
#197=ADVANCED_BREP_SHAPE_REPRESENTATION('',(#209),#3831);
#198=STYLED_ITEM('',(#3902),#204);
#199=STYLED_ITEM('',(#3903),#205);
#200=STYLED_ITEM('',(#3904),#206);
#201=STYLED_ITEM('',(#3905),#207);
#202=STYLED_ITEM('',(#3905),#208);
#203=STYLED_ITEM('',(#3906),#209);
#204=MANIFOLD_SOLID_BREP('Body1',#1783);
#205=MANIFOLD_SOLID_BREP('Body1',#1784);
#206=MANIFOLD_SOLID_BREP('Body1',#1785);
#207=MANIFOLD_SOLID_BREP('Body1',#1786);
#208=MANIFOLD_SOLID_BREP('Body1',#1787);
#209=MANIFOLD_SOLID_BREP('Body1',#1788);
#210=FACE_BOUND('',#381,.T.);
#211=FACE_BOUND('',#383,.T.);
#212=FACE_BOUND('',#386,.T.);
#213=FACE_BOUND('',#388,.T.);
#214=FACE_BOUND('',#393,.T.);
#215=FACE_BOUND('',#394,.T.);
#216=FACE_BOUND('',#395,.T.);
#217=FACE_BOUND('',#396,.T.);
#218=FACE_BOUND('',#397,.T.);
#219=FACE_BOUND('',#399,.T.);
#220=FACE_BOUND('',#400,.T.);
#221=FACE_BOUND('',#401,.T.);
#222=FACE_BOUND('',#402,.T.);
#223=FACE_BOUND('',#403,.T.);
#224=FACE_BOUND('',#436,.T.);
#225=FACE_BOUND('',#454,.T.);
#226=FACE_BOUND('',#457,.T.);
#227=PLANE('',#1867);
#228=PLANE('',#1868);
#229=PLANE('',#1872);
#230=PLANE('',#1873);
#231=PLANE('',#1878);
#232=PLANE('',#1879);
#233=PLANE('',#1881);
#234=PLANE('',#1890);
#235=PLANE('',#1899);
#236=PLANE('',#1901);
#237=PLANE('',#1903);
#238=PLANE('',#1905);
#239=PLANE('',#1911);
#240=PLANE('',#1912);
#241=PLANE('',#1913);
#242=PLANE('',#1914);
#243=PLANE('',#1916);
#244=PLANE('',#1917);
#245=PLANE('',#1918);
#246=PLANE('',#1919);
#247=PLANE('',#1920);
#248=PLANE('',#1921);
#249=PLANE('',#1934);
#250=PLANE('',#1941);
#251=PLANE('',#1946);
#252=PLANE('',#1952);
#253=PLANE('',#1953);
#254=PLANE('',#1954);
#255=PLANE('',#1955);
#256=PLANE('',#1956);
#257=PLANE('',#1957);
#258=PLANE('',#1958);
#259=PLANE('',#1970);
#260=PLANE('',#1990);
#261=PLANE('',#1996);
#262=PLANE('',#1997);
#263=PLANE('',#1999);
#264=PLANE('',#2007);
#265=PLANE('',#2011);
#266=PLANE('',#2013);
#267=PLANE('',#2014);
#268=PLANE('',#2015);
#269=PLANE('',#2020);
#270=PLANE('',#2024);
#271=PLANE('',#2029);
#272=PLANE('',#2032);
#273=FACE_OUTER_BOUND('',#377,.T.);
#274=FACE_OUTER_BOUND('',#378,.T.);
#275=FACE_OUTER_BOUND('',#379,.T.);
#276=FACE_OUTER_BOUND('',#380,.T.);
#277=FACE_OUTER_BOUND('',#382,.T.);
#278=FACE_OUTER_BOUND('',#384,.T.);
#279=FACE_OUTER_BOUND('',#385,.T.);
#280=FACE_OUTER_BOUND('',#387,.T.);
#281=FACE_OUTER_BOUND('',#389,.T.);
#282=FACE_OUTER_BOUND('',#390,.T.);
#283=FACE_OUTER_BOUND('',#391,.T.);
#284=FACE_OUTER_BOUND('',#392,.T.);
#285=FACE_OUTER_BOUND('',#398,.T.);
#286=FACE_OUTER_BOUND('',#404,.T.);
#287=FACE_OUTER_BOUND('',#405,.T.);
#288=FACE_OUTER_BOUND('',#406,.T.);
#289=FACE_OUTER_BOUND('',#407,.T.);
#290=FACE_OUTER_BOUND('',#408,.T.);
#291=FACE_OUTER_BOUND('',#409,.T.);
#292=FACE_OUTER_BOUND('',#410,.T.);
#293=FACE_OUTER_BOUND('',#411,.T.);
#294=FACE_OUTER_BOUND('',#412,.T.);
#295=FACE_OUTER_BOUND('',#413,.T.);
#296=FACE_OUTER_BOUND('',#414,.T.);
#297=FACE_OUTER_BOUND('',#415,.T.);
#298=FACE_OUTER_BOUND('',#416,.T.);
#299=FACE_OUTER_BOUND('',#417,.T.);
#300=FACE_OUTER_BOUND('',#418,.T.);
#301=FACE_OUTER_BOUND('',#419,.T.);
#302=FACE_OUTER_BOUND('',#420,.T.);
#303=FACE_OUTER_BOUND('',#421,.T.);
#304=FACE_OUTER_BOUND('',#422,.T.);
#305=FACE_OUTER_BOUND('',#423,.T.);
#306=FACE_OUTER_BOUND('',#424,.T.);
#307=FACE_OUTER_BOUND('',#425,.T.);
#308=FACE_OUTER_BOUND('',#426,.T.);
#309=FACE_OUTER_BOUND('',#427,.T.);
#310=FACE_OUTER_BOUND('',#428,.T.);
#311=FACE_OUTER_BOUND('',#429,.T.);
#312=FACE_OUTER_BOUND('',#430,.T.);
#313=FACE_OUTER_BOUND('',#431,.T.);
#314=FACE_OUTER_BOUND('',#432,.T.);
#315=FACE_OUTER_BOUND('',#433,.T.);
#316=FACE_OUTER_BOUND('',#434,.T.);
#317=FACE_OUTER_BOUND('',#435,.T.);
#318=FACE_OUTER_BOUND('',#437,.T.);
#319=FACE_OUTER_BOUND('',#438,.T.);
#320=FACE_OUTER_BOUND('',#439,.T.);
#321=FACE_OUTER_BOUND('',#440,.T.);
#322=FACE_OUTER_BOUND('',#441,.T.);
#323=FACE_OUTER_BOUND('',#442,.T.);
#324=FACE_OUTER_BOUND('',#443,.T.);
#325=FACE_OUTER_BOUND('',#444,.T.);
#326=FACE_OUTER_BOUND('',#445,.T.);
#327=FACE_OUTER_BOUND('',#446,.T.);
#328=FACE_OUTER_BOUND('',#447,.T.);
#329=FACE_OUTER_BOUND('',#448,.T.);
#330=FACE_OUTER_BOUND('',#449,.T.);
#331=FACE_OUTER_BOUND('',#450,.T.);
#332=FACE_OUTER_BOUND('',#451,.T.);
#333=FACE_OUTER_BOUND('',#452,.T.);
#334=FACE_OUTER_BOUND('',#453,.T.);
#335=FACE_OUTER_BOUND('',#455,.T.);
#336=FACE_OUTER_BOUND('',#456,.T.);
#337=FACE_OUTER_BOUND('',#458,.T.);
#338=FACE_OUTER_BOUND('',#459,.T.);
#339=FACE_OUTER_BOUND('',#460,.T.);
#340=FACE_OUTER_BOUND('',#461,.T.);
#341=FACE_OUTER_BOUND('',#462,.T.);
#342=FACE_OUTER_BOUND('',#463,.T.);
#343=FACE_OUTER_BOUND('',#464,.T.);
#344=FACE_OUTER_BOUND('',#465,.T.);
#345=FACE_OUTER_BOUND('',#466,.T.);
#346=FACE_OUTER_BOUND('',#467,.T.);
#347=FACE_OUTER_BOUND('',#468,.T.);
#348=FACE_OUTER_BOUND('',#469,.T.);
#349=FACE_OUTER_BOUND('',#470,.T.);
#350=FACE_OUTER_BOUND('',#471,.T.);
#351=FACE_OUTER_BOUND('',#472,.T.);
#352=FACE_OUTER_BOUND('',#473,.T.);
#353=FACE_OUTER_BOUND('',#474,.T.);
#354=FACE_OUTER_BOUND('',#475,.T.);
#355=FACE_OUTER_BOUND('',#476,.T.);
#356=FACE_OUTER_BOUND('',#477,.T.);
#357=FACE_OUTER_BOUND('',#478,.T.);
#358=FACE_OUTER_BOUND('',#479,.T.);
#359=FACE_OUTER_BOUND('',#480,.T.);
#360=FACE_OUTER_BOUND('',#481,.T.);
#361=FACE_OUTER_BOUND('',#482,.T.);
#362=FACE_OUTER_BOUND('',#483,.T.);
#363=FACE_OUTER_BOUND('',#484,.T.);
#364=FACE_OUTER_BOUND('',#485,.T.);
#365=FACE_OUTER_BOUND('',#486,.T.);
#366=FACE_OUTER_BOUND('',#487,.T.);
#367=FACE_OUTER_BOUND('',#488,.T.);
#368=FACE_OUTER_BOUND('',#489,.T.);
#369=FACE_OUTER_BOUND('',#490,.T.);
#370=FACE_OUTER_BOUND('',#491,.T.);
#371=FACE_OUTER_BOUND('',#492,.T.);
#372=FACE_OUTER_BOUND('',#493,.T.);
#373=FACE_OUTER_BOUND('',#494,.T.);
#374=FACE_OUTER_BOUND('',#495,.T.);
#375=FACE_OUTER_BOUND('',#496,.T.);
#376=FACE_OUTER_BOUND('',#497,.T.);
#377=EDGE_LOOP('',(#1153,#1154,#1155,#1156));
#378=EDGE_LOOP('',(#1157,#1158,#1159,#1160));
#379=EDGE_LOOP('',(#1161,#1162,#1163,#1164));
#380=EDGE_LOOP('',(#1165));
#381=EDGE_LOOP('',(#1166));
#382=EDGE_LOOP('',(#1167));
#383=EDGE_LOOP('',(#1168));
#384=EDGE_LOOP('',(#1169,#1170,#1171,#1172));
#385=EDGE_LOOP('',(#1173));
#386=EDGE_LOOP('',(#1174));
#387=EDGE_LOOP('',(#1175));
#388=EDGE_LOOP('',(#1176));
#389=EDGE_LOOP('',(#1177,#1178,#1179,#1180));
#390=EDGE_LOOP('',(#1181));
#391=EDGE_LOOP('',(#1182));
#392=EDGE_LOOP('',(#1183,#1184,#1185,#1186,#1187,#1188,#1189,#1190));
#393=EDGE_LOOP('',(#1191,#1192,#1193,#1194));
#394=EDGE_LOOP('',(#1195));
#395=EDGE_LOOP('',(#1196));
#396=EDGE_LOOP('',(#1197));
#397=EDGE_LOOP('',(#1198));
#398=EDGE_LOOP('',(#1199,#1200,#1201,#1202,#1203,#1204,#1205,#1206));
#399=EDGE_LOOP('',(#1207));
#400=EDGE_LOOP('',(#1208));
#401=EDGE_LOOP('',(#1209));
#402=EDGE_LOOP('',(#1210));
#403=EDGE_LOOP('',(#1211,#1212,#1213,#1214));
#404=EDGE_LOOP('',(#1215,#1216,#1217,#1218));
#405=EDGE_LOOP('',(#1219,#1220,#1221,#1222));
#406=EDGE_LOOP('',(#1223,#1224,#1225,#1226));
#407=EDGE_LOOP('',(#1227,#1228,#1229,#1230));
#408=EDGE_LOOP('',(#1231,#1232,#1233,#1234));
#409=EDGE_LOOP('',(#1235,#1236,#1237,#1238));
#410=EDGE_LOOP('',(#1239,#1240,#1241,#1242));
#411=EDGE_LOOP('',(#1243,#1244,#1245,#1246));
#412=EDGE_LOOP('',(#1247,#1248,#1249,#1250));
#413=EDGE_LOOP('',(#1251,#1252,#1253,#1254));
#414=EDGE_LOOP('',(#1255,#1256,#1257,#1258));
#415=EDGE_LOOP('',(#1259,#1260,#1261,#1262));
#416=EDGE_LOOP('',(#1263,#1264,#1265,#1266));
#417=EDGE_LOOP('',(#1267,#1268,#1269,#1270));
#418=EDGE_LOOP('',(#1271,#1272,#1273,#1274));
#419=EDGE_LOOP('',(#1275,#1276,#1277,#1278));
#420=EDGE_LOOP('',(#1279,#1280,#1281,#1282,#1283));
#421=EDGE_LOOP('',(#1284,#1285,#1286,#1287,#1288));
#422=EDGE_LOOP('',(#1289,#1290,#1291,#1292,#1293));
#423=EDGE_LOOP('',(#1294,#1295,#1296,#1297,#1298));
#424=EDGE_LOOP('',(#1299,#1300,#1301,#1302,#1303));
#425=EDGE_LOOP('',(#1304,#1305,#1306,#1307,#1308));
#426=EDGE_LOOP('',(#1309,#1310,#1311));
#427=EDGE_LOOP('',(#1312,#1313,#1314));
#428=EDGE_LOOP('',(#1315,#1316,#1317));
#429=EDGE_LOOP('',(#1318,#1319,#1320));
#430=EDGE_LOOP('',(#1321,#1322,#1323));
#431=EDGE_LOOP('',(#1324,#1325,#1326));
#432=EDGE_LOOP('',(#1327,#1328,#1329,#1330,#1331,#1332));
#433=EDGE_LOOP('',(#1333,#1334,#1335,#1336,#1337));
#434=EDGE_LOOP('',(#1338,#1339,#1340,#1341,#1342,#1343,#1344,#1345,#1346,
#1347));
#435=EDGE_LOOP('',(#1348));
#436=EDGE_LOOP('',(#1349));
#437=EDGE_LOOP('',(#1350,#1351,#1352,#1353));
#438=EDGE_LOOP('',(#1354,#1355,#1356,#1357));
#439=EDGE_LOOP('',(#1358,#1359,#1360,#1361));
#440=EDGE_LOOP('',(#1362,#1363,#1364,#1365));
#441=EDGE_LOOP('',(#1366,#1367,#1368,#1369));
#442=EDGE_LOOP('',(#1370,#1371,#1372,#1373));
#443=EDGE_LOOP('',(#1374,#1375,#1376,#1377));
#444=EDGE_LOOP('',(#1378));
#445=EDGE_LOOP('',(#1379,#1380,#1381,#1382));
#446=EDGE_LOOP('',(#1383,#1384,#1385,#1386));
#447=EDGE_LOOP('',(#1387,#1388,#1389,#1390,#1391));
#448=EDGE_LOOP('',(#1392,#1393,#1394,#1395,#1396));
#449=EDGE_LOOP('',(#1397,#1398,#1399,#1400,#1401));
#450=EDGE_LOOP('',(#1402,#1403,#1404,#1405,#1406));
#451=EDGE_LOOP('',(#1407,#1408,#1409,#1410,#1411));
#452=EDGE_LOOP('',(#1412,#1413,#1414,#1415,#1416));
#453=EDGE_LOOP('',(#1417,#1418,#1419,#1420,#1421,#1422));
#454=EDGE_LOOP('',(#1423));
#455=EDGE_LOOP('',(#1424,#1425,#1426,#1427,#1428));
#456=EDGE_LOOP('',(#1429));
#457=EDGE_LOOP('',(#1430));
#458=EDGE_LOOP('',(#1431,#1432,#1433));
#459=EDGE_LOOP('',(#1434,#1435,#1436));
#460=EDGE_LOOP('',(#1437,#1438,#1439));
#461=EDGE_LOOP('',(#1440,#1441,#1442));
#462=EDGE_LOOP('',(#1443,#1444,#1445));
#463=EDGE_LOOP('',(#1446,#1447,#1448));
#464=EDGE_LOOP('',(#1449,#1450,#1451,#1452,#1453,#1454,#1455,#1456,#1457,
#1458));
#465=EDGE_LOOP('',(#1459,#1460,#1461,#1462,#1463));
#466=EDGE_LOOP('',(#1464,#1465,#1466,#1467));
#467=EDGE_LOOP('',(#1468,#1469,#1470,#1471));
#468=EDGE_LOOP('',(#1472,#1473,#1474,#1475));
#469=EDGE_LOOP('',(#1476,#1477,#1478,#1479));
#470=EDGE_LOOP('',(#1480,#1481,#1482,#1483));
#471=EDGE_LOOP('',(#1484,#1485,#1486,#1487));
#472=EDGE_LOOP('',(#1488,#1489,#1490,#1491));
#473=EDGE_LOOP('',(#1492,#1493,#1494,#1495,#1496));
#474=EDGE_LOOP('',(#1497,#1498,#1499,#1500,#1501,#1502,#1503,#1504));
#475=EDGE_LOOP('',(#1505,#1506));
#476=EDGE_LOOP('',(#1507,#1508,#1509,#1510,#1511,#1512,#1513,#1514,#1515,
#1516));
#477=EDGE_LOOP('',(#1517,#1518,#1519,#1520,#1521,#1522,#1523,#1524));
#478=EDGE_LOOP('',(#1525,#1526));
#479=EDGE_LOOP('',(#1527,#1528));
#480=EDGE_LOOP('',(#1529,#1530,#1531,#1532,#1533,#1534,#1535,#1536,#1537));
#481=EDGE_LOOP('',(#1538,#1539,#1540,#1541,#1542,#1543,#1544,#1545,#1546));
#482=EDGE_LOOP('',(#1547,#1548,#1549,#1550,#1551,#1552));
#483=EDGE_LOOP('',(#1553,#1554,#1555,#1556));
#484=EDGE_LOOP('',(#1557,#1558,#1559,#1560,#1561,#1562));
#485=EDGE_LOOP('',(#1563,#1564,#1565,#1566));
#486=EDGE_LOOP('',(#1567,#1568,#1569,#1570));
#487=EDGE_LOOP('',(#1571,#1572,#1573,#1574,#1575,#1576,#1577,#1578,#1579,
#1580,#1581,#1582));
#488=EDGE_LOOP('',(#1583,#1584,#1585,#1586,#1587,#1588,#1589,#1590));
#489=EDGE_LOOP('',(#1591,#1592,#1593,#1594,#1595,#1596,#1597,#1598));
#490=EDGE_LOOP('',(#1599,#1600,#1601,#1602,#1603,#1604,#1605,#1606,#1607,
#1608,#1609));
#491=EDGE_LOOP('',(#1610,#1611,#1612,#1613,#1614));
#492=EDGE_LOOP('',(#1615,#1616,#1617,#1618,#1619,#1620,#1621,#1622));
#493=EDGE_LOOP('',(#1623,#1624));
#494=EDGE_LOOP('',(#1625,#1626,#1627,#1628,#1629,#1630,#1631,#1632,#1633,
#1634));
#495=EDGE_LOOP('',(#1635,#1636,#1637,#1638,#1639,#1640,#1641,#1642));
#496=EDGE_LOOP('',(#1643,#1644,#1645,#1646,#1647));
#497=EDGE_LOOP('',(#1648,#1649,#1650,#1651,#1652));
#498=LINE('',#2531,#591);
#499=LINE('',#2537,#592);
#500=LINE('',#2543,#593);
#501=LINE('',#2551,#594);
#502=LINE('',#2560,#595);
#503=LINE('',#2568,#596);
#504=LINE('',#2572,#597);
#505=LINE('',#2576,#598);
#506=LINE('',#2580,#599);
#507=LINE('',#2584,#600);
#508=LINE('',#2586,#601);
#509=LINE('',#2588,#602);
#510=LINE('',#2589,#603);
#511=LINE('',#2601,#604);
#512=LINE('',#2605,#605);
#513=LINE('',#2609,#606);
#514=LINE('',#2613,#607);
#515=LINE('',#2625,#608);
#516=LINE('',#2627,#609);
#517=LINE('',#2629,#610);
#518=LINE('',#2630,#611);
#519=LINE('',#2632,#612);
#520=LINE('',#2633,#613);
#521=LINE('',#2635,#614);
#522=LINE('',#2637,#615);
#523=LINE('',#2639,#616);
#524=LINE('',#2641,#617);
#525=LINE('',#2643,#618);
#526=LINE('',#2645,#619);
#527=LINE('',#2647,#620);
#528=LINE('',#2649,#621);
#529=LINE('',#2651,#622);
#530=LINE('',#2653,#623);
#531=LINE('',#2656,#624);
#532=LINE('',#2657,#625);
#533=LINE('',#2659,#626);
#534=LINE('',#2661,#627);
#535=LINE('',#2667,#628);
#536=LINE('',#2686,#629);
#537=LINE('',#2713,#630);
#538=LINE('',#2740,#631);
#539=LINE('',#2767,#632);
#540=LINE('',#2794,#633);
#541=LINE('',#2849,#634);
#542=LINE('',#3054,#635);
#543=LINE('',#3062,#636);
#544=LINE('',#3067,#637);
#545=LINE('',#3086,#638);
#546=LINE('',#3113,#639);
#547=LINE('',#3140,#640);
#548=LINE('',#3167,#641);
#549=LINE('',#3194,#642);
#550=LINE('',#3240,#643);
#551=LINE('',#3259,#644);
#552=LINE('',#3461,#645);
#553=LINE('',#3463,#646);
#554=LINE('',#3499,#647);
#555=LINE('',#3538,#648);
#556=LINE('',#3568,#649);
#557=LINE('',#3570,#650);
#558=LINE('',#3574,#651);
#559=LINE('',#3576,#652);
#560=LINE('',#3578,#653);
#561=LINE('',#3580,#654);
#562=LINE('',#3581,#655);
#563=LINE('',#3585,#656);
#564=LINE('',#3591,#657);
#565=LINE('',#3619,#658);
#566=LINE('',#3620,#659);
#567=LINE('',#3626,#660);
#568=LINE('',#3662,#661);
#569=LINE('',#3688,#662);
#570=LINE('',#3689,#663);
#571=LINE('',#3690,#664);
#572=LINE('',#3696,#665);
#573=LINE('',#3698,#666);
#574=LINE('',#3699,#667);
#575=LINE('',#3703,#668);
#576=LINE('',#3705,#669);
#577=LINE('',#3706,#670);
#578=LINE('',#3709,#671);
#579=LINE('',#3710,#672);
#580=LINE('',#3713,#673);
#581=LINE('',#3716,#674);
#582=LINE('',#3717,#675);
#583=LINE('',#3719,#676);
#584=LINE('',#3722,#677);
#585=LINE('',#3755,#678);
#586=LINE('',#3761,#679);
#587=LINE('',#3794,#680);
#588=LINE('',#3797,#681);
#589=LINE('',#3798,#682);
#590=LINE('',#3801,#683);
#591=VECTOR('',#2056,0.0254);
#592=VECTOR('',#2063,0.0254);
#593=VECTOR('',#2070,0.0381);
#594=VECTOR('',#2081,0.00762);
#595=VECTOR('',#2094,0.00762);
#596=VECTOR('',#2105,1.);
#597=VECTOR('',#2108,1.);
#598=VECTOR('',#2111,1.);
#599=VECTOR('',#2114,1.);
#600=VECTOR('',#2117,1.);
#601=VECTOR('',#2118,1.);
#602=VECTOR('',#2119,1.);
#603=VECTOR('',#2120,1.);
#604=VECTOR('',#2131,1.);
#605=VECTOR('',#2134,1.);
#606=VECTOR('',#2137,1.);
#607=VECTOR('',#2140,1.);
#608=VECTOR('',#2151,1.);
#609=VECTOR('',#2152,1.);
#610=VECTOR('',#2153,1.);
#611=VECTOR('',#2154,1.);
#612=VECTOR('',#2157,1.);
#613=VECTOR('',#2158,1.);
#614=VECTOR('',#2161,1.);
#615=VECTOR('',#2164,1.);
#616=VECTOR('',#2167,1.);
#617=VECTOR('',#2170,1.);
#618=VECTOR('',#2173,1.);
#619=VECTOR('',#2176,1.);
#620=VECTOR('',#2179,0.0045);
#621=VECTOR('',#2182,0.0045);
#622=VECTOR('',#2185,0.0045);
#623=VECTOR('',#2188,0.0045);
#624=VECTOR('',#2193,1.);
#625=VECTOR('',#2194,1.);
#626=VECTOR('',#2197,1.);
#627=VECTOR('',#2200,1.);
#628=VECTOR('',#2207,1.);
#629=VECTOR('',#2208,1.);
#630=VECTOR('',#2211,1.);
#631=VECTOR('',#2214,1.);
#632=VECTOR('',#2217,1.);
#633=VECTOR('',#2220,1.);
#634=VECTOR('',#2261,1.);
#635=VECTOR('',#2270,0.003);
#636=VECTOR('',#2283,0.002458734125);
#637=VECTOR('',#2288,1.);
#638=VECTOR('',#2289,1.);
#639=VECTOR('',#2292,1.);
#640=VECTOR('',#2295,1.);
#641=VECTOR('',#2298,1.);
#642=VECTOR('',#2301,1.);
#643=VECTOR('',#2324,0.0024585);
#644=VECTOR('',#2351,0.00672685951651014);
#645=VECTOR('',#2360,0.003);
#646=VECTOR('',#2363,0.0024585);
#647=VECTOR('',#2370,0.00762);
#648=VECTOR('',#2375,1.);
#649=VECTOR('',#2384,1.);
#650=VECTOR('',#2385,1.);
#651=VECTOR('',#2390,1.);
#652=VECTOR('',#2391,1.);
#653=VECTOR('',#2392,1.);
#654=VECTOR('',#2393,1.);
#655=VECTOR('',#2394,1.);
#656=VECTOR('',#2397,1.);
#657=VECTOR('',#2404,1.);
#658=VECTOR('',#2411,1.);
#659=VECTOR('',#2412,1.);
#660=VECTOR('',#2417,1.);
#661=VECTOR('',#2418,1.);
#662=VECTOR('',#2423,1.);
#663=VECTOR('',#2424,1.);
#664=VECTOR('',#2425,1.);
#665=VECTOR('',#2432,1.);
#666=VECTOR('',#2435,1.);
#667=VECTOR('',#2436,1.);
#668=VECTOR('',#2441,1.);
#669=VECTOR('',#2442,1.);
#670=VECTOR('',#2443,1.);
#671=VECTOR('',#2446,1.);
#672=VECTOR('',#2447,1.);
#673=VECTOR('',#2450,1.);
#674=VECTOR('',#2453,1.);
#675=VECTOR('',#2454,1.);
#676=VECTOR('',#2457,1.);
#677=VECTOR('',#2460,1.);
#678=VECTOR('',#2473,1.);
#679=VECTOR('',#2480,0.00762);
#680=VECTOR('',#2485,1.);
#681=VECTOR('',#2488,1.);
#682=VECTOR('',#2489,1.);
#683=VECTOR('',#2494,1.);
#684=CIRCLE('',#1859,0.0254);
#685=CIRCLE('',#1860,0.0254);
#686=CIRCLE('',#1862,0.0254);
#687=CIRCLE('',#1863,0.0254);
#688=CIRCLE('',#1865,0.0381);
#689=CIRCLE('',#1866,0.0381);
#690=CIRCLE('',#1870,0.00762);
#691=CIRCLE('',#1871,0.00762);
#692=CIRCLE('',#1876,0.00762);
#693=CIRCLE('',#1877,0.00762);
#694=CIRCLE('',#1882,0.01);
#695=CIRCLE('',#1883,0.0100000000000001);
#696=CIRCLE('',#1884,0.0100000000000001);
#697=CIRCLE('',#1885,0.01);
#698=CIRCLE('',#1886,0.0045);
#699=CIRCLE('',#1887,0.0045);
#700=CIRCLE('',#1888,0.0045);
#701=CIRCLE('',#1889,0.0045);
#702=CIRCLE('',#1891,0.01);
#703=CIRCLE('',#1892,0.0100000000000001);
#704=CIRCLE('',#1893,0.0100000000000001);
#705=CIRCLE('',#1894,0.01);
#706=CIRCLE('',#1895,0.0045);
#707=CIRCLE('',#1896,0.0045);
#708=CIRCLE('',#1897,0.0045);
#709=CIRCLE('',#1898,0.0045);
#710=CIRCLE('',#1923,0.004);
#711=CIRCLE('',#1925,0.004);
#712=CIRCLE('',#1927,0.004);
#713=CIRCLE('',#1929,0.004);
#714=CIRCLE('',#1931,0.004);
#715=CIRCLE('',#1933,0.004);
#716=CIRCLE('',#1936,0.00699395967877932);
#717=CIRCLE('',#1937,0.00699395967877932);
#718=CIRCLE('',#1938,0.000567100162269167);
#719=CIRCLE('',#1939,0.0068);
#720=CIRCLE('',#1942,0.00325);
#721=CIRCLE('',#1944,0.003);
#722=CIRCLE('',#1945,0.003);
#723=CIRCLE('',#1947,0.002458734125);
#724=CIRCLE('',#1949,0.00025);
#725=CIRCLE('',#1959,0.005);
#726=CIRCLE('',#1960,0.005);
#727=CIRCLE('',#1961,0.005);
#728=CIRCLE('',#1962,0.005);
#729=CIRCLE('',#1963,0.005);
#730=CIRCLE('',#1964,0.005);
#731=CIRCLE('',#1965,0.003);
#732=CIRCLE('',#1967,0.0024585);
#733=CIRCLE('',#1968,0.0024585);
#734=CIRCLE('',#1969,0.0024585);
#735=CIRCLE('',#1971,0.00653289983773083);
#736=CIRCLE('',#1972,0.003);
#737=CIRCLE('',#1980,0.00672685951651014);
#738=CIRCLE('',#1981,0.00672685951651014);
#739=CIRCLE('',#1983,0.000567100162269171);
#740=CIRCLE('',#1991,0.01508125);
#741=CIRCLE('',#1995,0.0608802828924915);
#742=CIRCLE('',#1998,0.01508125);
#743=CIRCLE('',#2000,0.01508125);
#744=CIRCLE('',#2019,0.01508125);
#745=CIRCLE('',#2031,0.0608802828794672);
#746=VERTEX_POINT('',#2528);
#747=VERTEX_POINT('',#2530);
#748=VERTEX_POINT('',#2534);
#749=VERTEX_POINT('',#2536);
#750=VERTEX_POINT('',#2540);
#751=VERTEX_POINT('',#2542);
#752=VERTEX_POINT('',#2548);
#753=VERTEX_POINT('',#2550);
#754=VERTEX_POINT('',#2557);
#755=VERTEX_POINT('',#2559);
#756=VERTEX_POINT('',#2566);
#757=VERTEX_POINT('',#2567);
#758=VERTEX_POINT('',#2569);
#759=VERTEX_POINT('',#2571);
#760=VERTEX_POINT('',#2573);
#761=VERTEX_POINT('',#2575);
#762=VERTEX_POINT('',#2577);
#763=VERTEX_POINT('',#2579);
#764=VERTEX_POINT('',#2582);
#765=VERTEX_POINT('',#2583);
#766=VERTEX_POINT('',#2585);
#767=VERTEX_POINT('',#2587);
#768=VERTEX_POINT('',#2590);
#769=VERTEX_POINT('',#2592);
#770=VERTEX_POINT('',#2594);
#771=VERTEX_POINT('',#2596);
#772=VERTEX_POINT('',#2599);
#773=VERTEX_POINT('',#2600);
#774=VERTEX_POINT('',#2602);
#775=VERTEX_POINT('',#2604);
#776=VERTEX_POINT('',#2606);
#777=VERTEX_POINT('',#2608);
#778=VERTEX_POINT('',#2610);
#779=VERTEX_POINT('',#2612);
#780=VERTEX_POINT('',#2615);
#781=VERTEX_POINT('',#2617);
#782=VERTEX_POINT('',#2619);
#783=VERTEX_POINT('',#2621);
#784=VERTEX_POINT('',#2623);
#785=VERTEX_POINT('',#2624);
#786=VERTEX_POINT('',#2626);
#787=VERTEX_POINT('',#2628);
#788=VERTEX_POINT('',#2665);
#789=VERTEX_POINT('',#2666);
#790=VERTEX_POINT('',#2668);
#791=VERTEX_POINT('',#2685);
#792=VERTEX_POINT('',#2687);
#793=VERTEX_POINT('',#2695);
#794=VERTEX_POINT('',#2712);
#795=VERTEX_POINT('',#2714);
#796=VERTEX_POINT('',#2722);
#797=VERTEX_POINT('',#2739);
#798=VERTEX_POINT('',#2741);
#799=VERTEX_POINT('',#2749);
#800=VERTEX_POINT('',#2766);
#801=VERTEX_POINT('',#2768);
#802=VERTEX_POINT('',#2776);
#803=VERTEX_POINT('',#2793);
#804=VERTEX_POINT('',#2795);
#805=VERTEX_POINT('',#2819);
#806=VERTEX_POINT('',#2840);
#807=VERTEX_POINT('',#2841);
#808=VERTEX_POINT('',#2844);
#809=VERTEX_POINT('',#2848);
#810=VERTEX_POINT('',#2850);
#811=VERTEX_POINT('',#2856);
#812=VERTEX_POINT('',#2862);
#813=VERTEX_POINT('',#2868);
#814=VERTEX_POINT('',#2874);
#815=VERTEX_POINT('',#2886);
#816=VERTEX_POINT('',#3051);
#817=VERTEX_POINT('',#3053);
#818=VERTEX_POINT('',#3057);
#819=VERTEX_POINT('',#3065);
#820=VERTEX_POINT('',#3066);
#821=VERTEX_POINT('',#3068);
#822=VERTEX_POINT('',#3085);
#823=VERTEX_POINT('',#3087);
#824=VERTEX_POINT('',#3095);
#825=VERTEX_POINT('',#3112);
#826=VERTEX_POINT('',#3114);
#827=VERTEX_POINT('',#3122);
#828=VERTEX_POINT('',#3139);
#829=VERTEX_POINT('',#3141);
#830=VERTEX_POINT('',#3149);
#831=VERTEX_POINT('',#3166);
#832=VERTEX_POINT('',#3168);
#833=VERTEX_POINT('',#3176);
#834=VERTEX_POINT('',#3193);
#835=VERTEX_POINT('',#3195);
#836=VERTEX_POINT('',#3219);
#837=VERTEX_POINT('',#3233);
#838=VERTEX_POINT('',#3236);
#839=VERTEX_POINT('',#3237);
#840=VERTEX_POINT('',#3239);
#841=VERTEX_POINT('',#3244);
#842=VERTEX_POINT('',#3246);
#843=VERTEX_POINT('',#3255);
#844=VERTEX_POINT('',#3256);
#845=VERTEX_POINT('',#3258);
#846=VERTEX_POINT('',#3260);
#847=VERTEX_POINT('',#3266);
#848=VERTEX_POINT('',#3272);
#849=VERTEX_POINT('',#3278);
#850=VERTEX_POINT('',#3284);
#851=VERTEX_POINT('',#3466);
#852=VERTEX_POINT('',#3467);
#853=VERTEX_POINT('',#3482);
#854=VERTEX_POINT('',#3498);
#855=VERTEX_POINT('',#3500);
#856=VERTEX_POINT('',#3517);
#857=VERTEX_POINT('',#3536);
#858=VERTEX_POINT('',#3537);
#859=VERTEX_POINT('',#3541);
#860=VERTEX_POINT('',#3542);
#861=VERTEX_POINT('',#3551);
#862=VERTEX_POINT('',#3566);
#863=VERTEX_POINT('',#3569);
#864=VERTEX_POINT('',#3573);
#865=VERTEX_POINT('',#3575);
#866=VERTEX_POINT('',#3577);
#867=VERTEX_POINT('',#3579);
#868=VERTEX_POINT('',#3583);
#869=VERTEX_POINT('',#3584);
#870=VERTEX_POINT('',#3588);
#871=VERTEX_POINT('',#3589);
#872=VERTEX_POINT('',#3593);
#873=VERTEX_POINT('',#3594);
#874=VERTEX_POINT('',#3610);
#875=VERTEX_POINT('',#3617);
#876=VERTEX_POINT('',#3622);
#877=VERTEX_POINT('',#3623);
#878=VERTEX_POINT('',#3625);
#879=VERTEX_POINT('',#3627);
#880=VERTEX_POINT('',#3644);
#881=VERTEX_POINT('',#3661);
#882=VERTEX_POINT('',#3663);
#883=VERTEX_POINT('',#3686);
#884=VERTEX_POINT('',#3687);
#885=VERTEX_POINT('',#3692);
#886=VERTEX_POINT('',#3694);
#887=VERTEX_POINT('',#3702);
#888=VERTEX_POINT('',#3704);
#889=VERTEX_POINT('',#3708);
#890=VERTEX_POINT('',#3712);
#891=VERTEX_POINT('',#3714);
#892=VERTEX_POINT('',#3721);
#893=VERTEX_POINT('',#3723);
#894=VERTEX_POINT('',#3731);
#895=VERTEX_POINT('',#3748);
#896=VERTEX_POINT('',#3749);
#897=VERTEX_POINT('',#3754);
#898=VERTEX_POINT('',#3756);
#899=VERTEX_POINT('',#3760);
#900=VERTEX_POINT('',#3762);
#901=VERTEX_POINT('',#3777);
#902=VERTEX_POINT('',#3796);
#903=EDGE_CURVE('',#746,#746,#684,.T.);
#904=EDGE_CURVE('',#746,#747,#498,.T.);
#905=EDGE_CURVE('',#747,#747,#685,.T.);
#906=EDGE_CURVE('',#748,#748,#686,.T.);
#907=EDGE_CURVE('',#748,#749,#499,.T.);
#908=EDGE_CURVE('',#749,#749,#687,.T.);
#909=EDGE_CURVE('',#750,#750,#688,.T.);
#910=EDGE_CURVE('',#750,#751,#500,.T.);
#911=EDGE_CURVE('',#751,#751,#689,.T.);
#912=EDGE_CURVE('',#752,#752,#690,.T.);
#913=EDGE_CURVE('',#752,#753,#501,.T.);
#914=EDGE_CURVE('',#753,#753,#691,.T.);
#915=EDGE_CURVE('',#754,#754,#692,.T.);
#916=EDGE_CURVE('',#754,#755,#502,.T.);
#917=EDGE_CURVE('',#755,#755,#693,.T.);
#918=EDGE_CURVE('',#756,#757,#503,.T.);
#919=EDGE_CURVE('',#758,#756,#694,.T.);
#920=EDGE_CURVE('',#758,#759,#504,.T.);
#921=EDGE_CURVE('',#760,#759,#695,.T.);
#922=EDGE_CURVE('',#760,#761,#505,.T.);
#923=EDGE_CURVE('',#762,#761,#696,.T.);
#924=EDGE_CURVE('',#763,#762,#506,.T.);
#925=EDGE_CURVE('',#757,#763,#697,.T.);
#926=EDGE_CURVE('',#764,#765,#507,.T.);
#927=EDGE_CURVE('',#765,#766,#508,.T.);
#928=EDGE_CURVE('',#767,#766,#509,.T.);
#929=EDGE_CURVE('',#764,#767,#510,.T.);
#930=EDGE_CURVE('',#768,#768,#698,.T.);
#931=EDGE_CURVE('',#769,#769,#699,.T.);
#932=EDGE_CURVE('',#770,#770,#700,.T.);
#933=EDGE_CURVE('',#771,#771,#701,.T.);
#934=EDGE_CURVE('',#772,#773,#511,.T.);
#935=EDGE_CURVE('',#773,#774,#702,.T.);
#936=EDGE_CURVE('',#774,#775,#512,.T.);
#937=EDGE_CURVE('',#775,#776,#703,.T.);
#938=EDGE_CURVE('',#777,#776,#513,.T.);
#939=EDGE_CURVE('',#777,#778,#704,.T.);
#940=EDGE_CURVE('',#779,#778,#514,.T.);
#941=EDGE_CURVE('',#779,#772,#705,.T.);
#942=EDGE_CURVE('',#780,#780,#706,.T.);
#943=EDGE_CURVE('',#781,#781,#707,.T.);
#944=EDGE_CURVE('',#782,#782,#708,.T.);
#945=EDGE_CURVE('',#783,#783,#709,.T.);
#946=EDGE_CURVE('',#784,#785,#515,.T.);
#947=EDGE_CURVE('',#786,#784,#516,.T.);
#948=EDGE_CURVE('',#786,#787,#517,.T.);
#949=EDGE_CURVE('',#787,#785,#518,.T.);
#950=EDGE_CURVE('',#756,#772,#519,.T.);
#951=EDGE_CURVE('',#757,#773,#520,.T.);
#952=EDGE_CURVE('',#763,#774,#521,.T.);
#953=EDGE_CURVE('',#762,#775,#522,.T.);
#954=EDGE_CURVE('',#761,#776,#523,.T.);
#955=EDGE_CURVE('',#760,#777,#524,.T.);
#956=EDGE_CURVE('',#759,#778,#525,.T.);
#957=EDGE_CURVE('',#758,#779,#526,.T.);
#958=EDGE_CURVE('',#771,#780,#527,.T.);
#959=EDGE_CURVE('',#770,#781,#528,.T.);
#960=EDGE_CURVE('',#769,#782,#529,.T.);
#961=EDGE_CURVE('',#768,#783,#530,.T.);
#962=EDGE_CURVE('',#765,#784,#531,.T.);
#963=EDGE_CURVE('',#766,#785,#532,.T.);
#964=EDGE_CURVE('',#767,#787,#533,.T.);
#965=EDGE_CURVE('',#764,#786,#534,.T.);
#966=EDGE_CURVE('',#788,#789,#535,.T.);
#967=EDGE_CURVE('',#789,#790,#134,.T.);
#968=EDGE_CURVE('',#791,#790,#536,.T.);
#969=EDGE_CURVE('',#791,#792,#110,.T.);
#970=EDGE_CURVE('',#792,#788,#111,.T.);
#971=EDGE_CURVE('',#790,#793,#135,.T.);
#972=EDGE_CURVE('',#794,#793,#537,.T.);
#973=EDGE_CURVE('',#794,#795,#112,.T.);
#974=EDGE_CURVE('',#795,#791,#113,.T.);
#975=EDGE_CURVE('',#793,#796,#136,.T.);
#976=EDGE_CURVE('',#797,#796,#538,.T.);
#977=EDGE_CURVE('',#797,#798,#114,.F.);
#978=EDGE_CURVE('',#798,#794,#115,.F.);
#979=EDGE_CURVE('',#796,#799,#137,.T.);
#980=EDGE_CURVE('',#800,#799,#539,.T.);
#981=EDGE_CURVE('',#800,#801,#116,.T.);
#982=EDGE_CURVE('',#801,#797,#117,.T.);
#983=EDGE_CURVE('',#799,#802,#138,.T.);
#984=EDGE_CURVE('',#803,#802,#540,.T.);
#985=EDGE_CURVE('',#803,#804,#118,.T.);
#986=EDGE_CURVE('',#804,#800,#119,.T.);
#987=EDGE_CURVE('',#802,#789,#139,.T.);
#988=EDGE_CURVE('',#788,#805,#120,.T.);
#989=EDGE_CURVE('',#805,#803,#121,.T.);
#990=EDGE_CURVE('',#804,#805,#710,.T.);
#991=EDGE_CURVE('',#805,#792,#711,.T.);
#992=EDGE_CURVE('',#801,#804,#712,.T.);
#993=EDGE_CURVE('',#798,#801,#713,.T.);
#994=EDGE_CURVE('',#795,#798,#714,.T.);
#995=EDGE_CURVE('',#792,#795,#715,.T.);
#996=EDGE_CURVE('',#806,#807,#716,.T.);
#997=EDGE_CURVE('',#807,#806,#717,.T.);
#998=EDGE_CURVE('',#807,#808,#718,.T.);
#999=EDGE_CURVE('',#808,#808,#719,.T.);
#1000=EDGE_CURVE('',#806,#809,#541,.T.);
#1001=EDGE_CURVE('',#809,#810,#140,.T.);
#1002=EDGE_CURVE('',#810,#811,#141,.T.);
#1003=EDGE_CURVE('',#811,#812,#142,.T.);
#1004=EDGE_CURVE('',#812,#813,#143,.T.);
#1005=EDGE_CURVE('',#813,#814,#144,.T.);
#1006=EDGE_CURVE('',#814,#809,#145,.T.);
#1007=EDGE_CURVE('',#815,#815,#720,.T.);
#1008=EDGE_CURVE('',#799,#809,#146,.T.);
#1009=EDGE_CURVE('',#810,#796,#147,.F.);
#1010=EDGE_CURVE('',#811,#793,#148,.F.);
#1011=EDGE_CURVE('',#802,#814,#149,.T.);
#1012=EDGE_CURVE('',#812,#790,#150,.F.);
#1013=EDGE_CURVE('',#789,#813,#151,.T.);
#1014=EDGE_CURVE('',#816,#816,#721,.F.);
#1015=EDGE_CURVE('',#816,#817,#542,.T.);
#1016=EDGE_CURVE('',#817,#817,#722,.F.);
#1017=EDGE_CURVE('',#818,#818,#723,.T.);
#1018=EDGE_CURVE('',#815,#816,#724,.T.);
#1019=EDGE_CURVE('',#817,#818,#543,.T.);
#1020=EDGE_CURVE('',#819,#820,#544,.T.);
#1021=EDGE_CURVE('',#820,#821,#152,.T.);
#1022=EDGE_CURVE('',#822,#821,#545,.T.);
#1023=EDGE_CURVE('',#822,#823,#122,.T.);
#1024=EDGE_CURVE('',#823,#819,#123,.T.);
#1025=EDGE_CURVE('',#821,#824,#153,.T.);
#1026=EDGE_CURVE('',#825,#824,#546,.T.);
#1027=EDGE_CURVE('',#825,#826,#124,.T.);
#1028=EDGE_CURVE('',#826,#822,#125,.T.);
#1029=EDGE_CURVE('',#824,#827,#154,.T.);
#1030=EDGE_CURVE('',#828,#827,#547,.T.);
#1031=EDGE_CURVE('',#828,#829,#126,.T.);
#1032=EDGE_CURVE('',#829,#825,#127,.T.);
#1033=EDGE_CURVE('',#827,#830,#155,.T.);
#1034=EDGE_CURVE('',#831,#830,#548,.T.);
#1035=EDGE_CURVE('',#831,#832,#128,.F.);
#1036=EDGE_CURVE('',#832,#828,#129,.F.);
#1037=EDGE_CURVE('',#830,#833,#156,.T.);
#1038=EDGE_CURVE('',#834,#833,#549,.T.);
#1039=EDGE_CURVE('',#834,#835,#130,.T.);
#1040=EDGE_CURVE('',#835,#831,#131,.T.);
#1041=EDGE_CURVE('',#833,#820,#157,.T.);
#1042=EDGE_CURVE('',#819,#836,#132,.T.);
#1043=EDGE_CURVE('',#836,#834,#133,.T.);
#1044=EDGE_CURVE('',#835,#836,#725,.T.);
#1045=EDGE_CURVE('',#836,#823,#726,.T.);
#1046=EDGE_CURVE('',#823,#826,#727,.T.);
#1047=EDGE_CURVE('',#826,#829,#728,.T.);
#1048=EDGE_CURVE('',#829,#832,#729,.T.);
#1049=EDGE_CURVE('',#832,#835,#730,.T.);
#1050=EDGE_CURVE('',#837,#837,#731,.F.);
#1051=EDGE_CURVE('',#838,#839,#732,.T.);
#1052=EDGE_CURVE('',#839,#840,#550,.T.);
#1053=EDGE_CURVE('',#840,#840,#733,.F.);
#1054=EDGE_CURVE('',#839,#838,#734,.T.);
#1055=EDGE_CURVE('',#841,#841,#735,.T.);
#1056=EDGE_CURVE('',#842,#842,#736,.T.);
#1057=EDGE_CURVE('',#843,#844,#737,.T.);
#1058=EDGE_CURVE('',#844,#845,#551,.T.);
#1059=EDGE_CURVE('',#845,#846,#158,.T.);
#1060=EDGE_CURVE('',#846,#847,#159,.T.);
#1061=EDGE_CURVE('',#847,#848,#160,.T.);
#1062=EDGE_CURVE('',#848,#849,#161,.T.);
#1063=EDGE_CURVE('',#849,#850,#162,.T.);
#1064=EDGE_CURVE('',#850,#845,#163,.T.);
#1065=EDGE_CURVE('',#844,#843,#738,.T.);
#1066=EDGE_CURVE('',#843,#841,#739,.T.);
#1067=EDGE_CURVE('',#847,#827,#164,.F.);
#1068=EDGE_CURVE('',#830,#846,#165,.T.);
#1069=EDGE_CURVE('',#833,#845,#166,.T.);
#1070=EDGE_CURVE('',#848,#824,#167,.F.);
#1071=EDGE_CURVE('',#820,#850,#168,.T.);
#1072=EDGE_CURVE('',#849,#821,#169,.F.);
#1073=EDGE_CURVE('',#840,#842,#552,.T.);
#1074=EDGE_CURVE('',#838,#837,#553,.T.);
#1075=EDGE_CURVE('',#851,#852,#170,.T.);
#1076=EDGE_CURVE('',#853,#851,#59,.T.);
#1077=EDGE_CURVE('',#852,#853,#171,.T.);
#1078=EDGE_CURVE('',#852,#854,#554,.T.);
#1079=EDGE_CURVE('',#854,#855,#172,.F.);
#1080=EDGE_CURVE('',#856,#855,#60,.T.);
#1081=EDGE_CURVE('',#856,#854,#173,.F.);
#1082=EDGE_CURVE('',#857,#858,#555,.T.);
#1083=EDGE_CURVE('',#857,#858,#740,.T.);
#1084=EDGE_CURVE('',#859,#860,#61,.T.);
#1085=EDGE_CURVE('',#857,#860,#174,.T.);
#1086=EDGE_CURVE('',#861,#858,#175,.T.);
#1087=EDGE_CURVE('',#861,#862,#62,.T.);
#1088=EDGE_CURVE('',#851,#862,#556,.T.);
#1089=EDGE_CURVE('',#863,#853,#557,.T.);
#1090=EDGE_CURVE('',#859,#863,#741,.T.);
#1091=EDGE_CURVE('',#862,#864,#558,.T.);
#1092=EDGE_CURVE('',#864,#865,#559,.T.);
#1093=EDGE_CURVE('',#865,#866,#560,.T.);
#1094=EDGE_CURVE('',#867,#866,#561,.T.);
#1095=EDGE_CURVE('',#863,#867,#562,.F.);
#1096=EDGE_CURVE('',#868,#869,#563,.T.);
#1097=EDGE_CURVE('',#868,#869,#742,.T.);
#1098=EDGE_CURVE('',#870,#871,#743,.T.);
#1099=EDGE_CURVE('',#871,#870,#564,.T.);
#1100=EDGE_CURVE('',#872,#873,#63,.T.);
#1101=EDGE_CURVE('',#872,#870,#176,.T.);
#1102=EDGE_CURVE('',#871,#874,#177,.T.);
#1103=EDGE_CURVE('',#875,#874,#64,.T.);
#1104=EDGE_CURVE('',#875,#855,#565,.T.);
#1105=EDGE_CURVE('',#856,#873,#566,.T.);
#1106=EDGE_CURVE('',#876,#877,#65,.T.);
#1107=EDGE_CURVE('',#878,#876,#567,.T.);
#1108=EDGE_CURVE('',#879,#878,#178,.F.);
#1109=EDGE_CURVE('',#880,#879,#179,.F.);
#1110=EDGE_CURVE('',#881,#880,#568,.T.);
#1111=EDGE_CURVE('',#882,#881,#66,.T.);
#1112=EDGE_CURVE('',#882,#868,#180,.T.);
#1113=EDGE_CURVE('',#869,#877,#181,.T.);
#1114=EDGE_CURVE('',#883,#884,#569,.T.);
#1115=EDGE_CURVE('',#884,#873,#570,.T.);
#1116=EDGE_CURVE('',#875,#883,#571,.T.);
#1117=EDGE_CURVE('',#884,#885,#67,.T.);
#1118=EDGE_CURVE('',#886,#883,#68,.T.);
#1119=EDGE_CURVE('',#886,#885,#572,.T.);
#1120=EDGE_CURVE('',#885,#876,#573,.T.);
#1121=EDGE_CURVE('',#881,#886,#574,.T.);
#1122=EDGE_CURVE('',#878,#880,#69,.T.);
#1123=EDGE_CURVE('',#865,#887,#575,.T.);
#1124=EDGE_CURVE('',#888,#887,#576,.T.);
#1125=EDGE_CURVE('',#866,#888,#577,.T.);
#1126=EDGE_CURVE('',#864,#889,#578,.T.);
#1127=EDGE_CURVE('',#887,#889,#579,.T.);
#1128=EDGE_CURVE('',#877,#890,#580,.T.);
#1129=EDGE_CURVE('',#891,#890,#70,.T.);
#1130=EDGE_CURVE('',#889,#891,#581,.T.);
#1131=EDGE_CURVE('',#861,#872,#582,.T.);
#1132=EDGE_CURVE('',#860,#874,#583,.T.);
#1133=EDGE_CURVE('',#882,#892,#584,.T.);
#1134=EDGE_CURVE('',#892,#893,#182,.T.);
#1135=EDGE_CURVE('',#894,#893,#744,.T.);
#1136=EDGE_CURVE('',#894,#890,#183,.T.);
#1137=EDGE_CURVE('',#895,#896,#71,.T.);
#1138=EDGE_CURVE('',#892,#895,#72,.T.);
#1139=EDGE_CURVE('',#896,#859,#73,.T.);
#1140=EDGE_CURVE('',#897,#888,#585,.T.);
#1141=EDGE_CURVE('',#898,#897,#74,.F.);
#1142=EDGE_CURVE('',#867,#898,#75,.F.);
#1143=EDGE_CURVE('',#879,#899,#586,.T.);
#1144=EDGE_CURVE('',#900,#899,#184,.T.);
#1145=EDGE_CURVE('',#901,#900,#76,.T.);
#1146=EDGE_CURVE('',#899,#901,#185,.T.);
#1147=EDGE_CURVE('',#893,#894,#587,.T.);
#1148=EDGE_CURVE('',#902,#900,#588,.T.);
#1149=EDGE_CURVE('',#901,#891,#589,.T.);
#1150=EDGE_CURVE('',#902,#895,#745,.F.);
#1151=EDGE_CURVE('',#897,#902,#590,.F.);
#1152=EDGE_CURVE('',#896,#898,#77,.F.);
#1153=ORIENTED_EDGE('',*,*,#903,.T.);
#1154=ORIENTED_EDGE('',*,*,#904,.T.);
#1155=ORIENTED_EDGE('',*,*,#905,.F.);
#1156=ORIENTED_EDGE('',*,*,#904,.F.);
#1157=ORIENTED_EDGE('',*,*,#906,.T.);
#1158=ORIENTED_EDGE('',*,*,#907,.T.);
#1159=ORIENTED_EDGE('',*,*,#908,.F.);
#1160=ORIENTED_EDGE('',*,*,#907,.F.);
#1161=ORIENTED_EDGE('',*,*,#909,.T.);
#1162=ORIENTED_EDGE('',*,*,#910,.T.);
#1163=ORIENTED_EDGE('',*,*,#911,.F.);
#1164=ORIENTED_EDGE('',*,*,#910,.F.);
#1165=ORIENTED_EDGE('',*,*,#911,.T.);
#1166=ORIENTED_EDGE('',*,*,#906,.F.);
#1167=ORIENTED_EDGE('',*,*,#909,.F.);
#1168=ORIENTED_EDGE('',*,*,#905,.T.);
#1169=ORIENTED_EDGE('',*,*,#912,.T.);
#1170=ORIENTED_EDGE('',*,*,#913,.T.);
#1171=ORIENTED_EDGE('',*,*,#914,.F.);
#1172=ORIENTED_EDGE('',*,*,#913,.F.);
#1173=ORIENTED_EDGE('',*,*,#908,.T.);
#1174=ORIENTED_EDGE('',*,*,#912,.F.);
#1175=ORIENTED_EDGE('',*,*,#903,.F.);
#1176=ORIENTED_EDGE('',*,*,#914,.T.);
#1177=ORIENTED_EDGE('',*,*,#915,.T.);
#1178=ORIENTED_EDGE('',*,*,#916,.T.);
#1179=ORIENTED_EDGE('',*,*,#917,.F.);
#1180=ORIENTED_EDGE('',*,*,#916,.F.);
#1181=ORIENTED_EDGE('',*,*,#917,.T.);
#1182=ORIENTED_EDGE('',*,*,#915,.F.);
#1183=ORIENTED_EDGE('',*,*,#918,.F.);
#1184=ORIENTED_EDGE('',*,*,#919,.F.);
#1185=ORIENTED_EDGE('',*,*,#920,.T.);
#1186=ORIENTED_EDGE('',*,*,#921,.F.);
#1187=ORIENTED_EDGE('',*,*,#922,.T.);
#1188=ORIENTED_EDGE('',*,*,#923,.F.);
#1189=ORIENTED_EDGE('',*,*,#924,.F.);
#1190=ORIENTED_EDGE('',*,*,#925,.F.);
#1191=ORIENTED_EDGE('',*,*,#926,.T.);
#1192=ORIENTED_EDGE('',*,*,#927,.T.);
#1193=ORIENTED_EDGE('',*,*,#928,.F.);
#1194=ORIENTED_EDGE('',*,*,#929,.F.);
#1195=ORIENTED_EDGE('',*,*,#930,.T.);
#1196=ORIENTED_EDGE('',*,*,#931,.T.);
#1197=ORIENTED_EDGE('',*,*,#932,.T.);
#1198=ORIENTED_EDGE('',*,*,#933,.T.);
#1199=ORIENTED_EDGE('',*,*,#934,.T.);
#1200=ORIENTED_EDGE('',*,*,#935,.T.);
#1201=ORIENTED_EDGE('',*,*,#936,.T.);
#1202=ORIENTED_EDGE('',*,*,#937,.T.);
#1203=ORIENTED_EDGE('',*,*,#938,.F.);
#1204=ORIENTED_EDGE('',*,*,#939,.T.);
#1205=ORIENTED_EDGE('',*,*,#940,.F.);
#1206=ORIENTED_EDGE('',*,*,#941,.T.);
#1207=ORIENTED_EDGE('',*,*,#942,.F.);
#1208=ORIENTED_EDGE('',*,*,#943,.F.);
#1209=ORIENTED_EDGE('',*,*,#944,.F.);
#1210=ORIENTED_EDGE('',*,*,#945,.F.);
#1211=ORIENTED_EDGE('',*,*,#946,.F.);
#1212=ORIENTED_EDGE('',*,*,#947,.F.);
#1213=ORIENTED_EDGE('',*,*,#948,.T.);
#1214=ORIENTED_EDGE('',*,*,#949,.T.);
#1215=ORIENTED_EDGE('',*,*,#934,.F.);
#1216=ORIENTED_EDGE('',*,*,#950,.F.);
#1217=ORIENTED_EDGE('',*,*,#918,.T.);
#1218=ORIENTED_EDGE('',*,*,#951,.T.);
#1219=ORIENTED_EDGE('',*,*,#935,.F.);
#1220=ORIENTED_EDGE('',*,*,#951,.F.);
#1221=ORIENTED_EDGE('',*,*,#925,.T.);
#1222=ORIENTED_EDGE('',*,*,#952,.T.);
#1223=ORIENTED_EDGE('',*,*,#936,.F.);
#1224=ORIENTED_EDGE('',*,*,#952,.F.);
#1225=ORIENTED_EDGE('',*,*,#924,.T.);
#1226=ORIENTED_EDGE('',*,*,#953,.T.);
#1227=ORIENTED_EDGE('',*,*,#937,.F.);
#1228=ORIENTED_EDGE('',*,*,#953,.F.);
#1229=ORIENTED_EDGE('',*,*,#923,.T.);
#1230=ORIENTED_EDGE('',*,*,#954,.T.);
#1231=ORIENTED_EDGE('',*,*,#938,.T.);
#1232=ORIENTED_EDGE('',*,*,#954,.F.);
#1233=ORIENTED_EDGE('',*,*,#922,.F.);
#1234=ORIENTED_EDGE('',*,*,#955,.T.);
#1235=ORIENTED_EDGE('',*,*,#939,.F.);
#1236=ORIENTED_EDGE('',*,*,#955,.F.);
#1237=ORIENTED_EDGE('',*,*,#921,.T.);
#1238=ORIENTED_EDGE('',*,*,#956,.T.);
#1239=ORIENTED_EDGE('',*,*,#940,.T.);
#1240=ORIENTED_EDGE('',*,*,#956,.F.);
#1241=ORIENTED_EDGE('',*,*,#920,.F.);
#1242=ORIENTED_EDGE('',*,*,#957,.T.);
#1243=ORIENTED_EDGE('',*,*,#933,.F.);
#1244=ORIENTED_EDGE('',*,*,#958,.T.);
#1245=ORIENTED_EDGE('',*,*,#942,.T.);
#1246=ORIENTED_EDGE('',*,*,#958,.F.);
#1247=ORIENTED_EDGE('',*,*,#932,.F.);
#1248=ORIENTED_EDGE('',*,*,#959,.T.);
#1249=ORIENTED_EDGE('',*,*,#943,.T.);
#1250=ORIENTED_EDGE('',*,*,#959,.F.);
#1251=ORIENTED_EDGE('',*,*,#931,.F.);
#1252=ORIENTED_EDGE('',*,*,#960,.T.);
#1253=ORIENTED_EDGE('',*,*,#944,.T.);
#1254=ORIENTED_EDGE('',*,*,#960,.F.);
#1255=ORIENTED_EDGE('',*,*,#930,.F.);
#1256=ORIENTED_EDGE('',*,*,#961,.T.);
#1257=ORIENTED_EDGE('',*,*,#945,.T.);
#1258=ORIENTED_EDGE('',*,*,#961,.F.);
#1259=ORIENTED_EDGE('',*,*,#941,.F.);
#1260=ORIENTED_EDGE('',*,*,#957,.F.);
#1261=ORIENTED_EDGE('',*,*,#919,.T.);
#1262=ORIENTED_EDGE('',*,*,#950,.T.);
#1263=ORIENTED_EDGE('',*,*,#962,.T.);
#1264=ORIENTED_EDGE('',*,*,#946,.T.);
#1265=ORIENTED_EDGE('',*,*,#963,.F.);
#1266=ORIENTED_EDGE('',*,*,#927,.F.);
#1267=ORIENTED_EDGE('',*,*,#928,.T.);
#1268=ORIENTED_EDGE('',*,*,#963,.T.);
#1269=ORIENTED_EDGE('',*,*,#949,.F.);
#1270=ORIENTED_EDGE('',*,*,#964,.F.);
#1271=ORIENTED_EDGE('',*,*,#929,.T.);
#1272=ORIENTED_EDGE('',*,*,#964,.T.);
#1273=ORIENTED_EDGE('',*,*,#948,.F.);
#1274=ORIENTED_EDGE('',*,*,#965,.F.);
#1275=ORIENTED_EDGE('',*,*,#965,.T.);
#1276=ORIENTED_EDGE('',*,*,#947,.T.);
#1277=ORIENTED_EDGE('',*,*,#962,.F.);
#1278=ORIENTED_EDGE('',*,*,#926,.F.);
#1279=ORIENTED_EDGE('',*,*,#966,.T.);
#1280=ORIENTED_EDGE('',*,*,#967,.T.);
#1281=ORIENTED_EDGE('',*,*,#968,.F.);
#1282=ORIENTED_EDGE('',*,*,#969,.T.);
#1283=ORIENTED_EDGE('',*,*,#970,.T.);
#1284=ORIENTED_EDGE('',*,*,#968,.T.);
#1285=ORIENTED_EDGE('',*,*,#971,.T.);
#1286=ORIENTED_EDGE('',*,*,#972,.F.);
#1287=ORIENTED_EDGE('',*,*,#973,.T.);
#1288=ORIENTED_EDGE('',*,*,#974,.T.);
#1289=ORIENTED_EDGE('',*,*,#972,.T.);
#1290=ORIENTED_EDGE('',*,*,#975,.T.);
#1291=ORIENTED_EDGE('',*,*,#976,.F.);
#1292=ORIENTED_EDGE('',*,*,#977,.T.);
#1293=ORIENTED_EDGE('',*,*,#978,.T.);
#1294=ORIENTED_EDGE('',*,*,#976,.T.);
#1295=ORIENTED_EDGE('',*,*,#979,.T.);
#1296=ORIENTED_EDGE('',*,*,#980,.F.);
#1297=ORIENTED_EDGE('',*,*,#981,.T.);
#1298=ORIENTED_EDGE('',*,*,#982,.T.);
#1299=ORIENTED_EDGE('',*,*,#980,.T.);
#1300=ORIENTED_EDGE('',*,*,#983,.T.);
#1301=ORIENTED_EDGE('',*,*,#984,.F.);
#1302=ORIENTED_EDGE('',*,*,#985,.T.);
#1303=ORIENTED_EDGE('',*,*,#986,.T.);
#1304=ORIENTED_EDGE('',*,*,#984,.T.);
#1305=ORIENTED_EDGE('',*,*,#987,.T.);
#1306=ORIENTED_EDGE('',*,*,#966,.F.);
#1307=ORIENTED_EDGE('',*,*,#988,.T.);
#1308=ORIENTED_EDGE('',*,*,#989,.T.);
#1309=ORIENTED_EDGE('',*,*,#989,.F.);
#1310=ORIENTED_EDGE('',*,*,#990,.F.);
#1311=ORIENTED_EDGE('',*,*,#985,.F.);
#1312=ORIENTED_EDGE('',*,*,#991,.F.);
#1313=ORIENTED_EDGE('',*,*,#988,.F.);
#1314=ORIENTED_EDGE('',*,*,#970,.F.);
#1315=ORIENTED_EDGE('',*,*,#986,.F.);
#1316=ORIENTED_EDGE('',*,*,#992,.F.);
#1317=ORIENTED_EDGE('',*,*,#981,.F.);
#1318=ORIENTED_EDGE('',*,*,#982,.F.);
#1319=ORIENTED_EDGE('',*,*,#993,.F.);
#1320=ORIENTED_EDGE('',*,*,#977,.F.);
#1321=ORIENTED_EDGE('',*,*,#994,.F.);
#1322=ORIENTED_EDGE('',*,*,#973,.F.);
#1323=ORIENTED_EDGE('',*,*,#978,.F.);
#1324=ORIENTED_EDGE('',*,*,#995,.F.);
#1325=ORIENTED_EDGE('',*,*,#969,.F.);
#1326=ORIENTED_EDGE('',*,*,#974,.F.);
#1327=ORIENTED_EDGE('',*,*,#992,.T.);
#1328=ORIENTED_EDGE('',*,*,#990,.T.);
#1329=ORIENTED_EDGE('',*,*,#991,.T.);
#1330=ORIENTED_EDGE('',*,*,#995,.T.);
#1331=ORIENTED_EDGE('',*,*,#994,.T.);
#1332=ORIENTED_EDGE('',*,*,#993,.T.);
#1333=ORIENTED_EDGE('',*,*,#996,.F.);
#1334=ORIENTED_EDGE('',*,*,#997,.F.);
#1335=ORIENTED_EDGE('',*,*,#998,.T.);
#1336=ORIENTED_EDGE('',*,*,#999,.T.);
#1337=ORIENTED_EDGE('',*,*,#998,.F.);
#1338=ORIENTED_EDGE('',*,*,#996,.T.);
#1339=ORIENTED_EDGE('',*,*,#997,.T.);
#1340=ORIENTED_EDGE('',*,*,#1000,.T.);
#1341=ORIENTED_EDGE('',*,*,#1001,.T.);
#1342=ORIENTED_EDGE('',*,*,#1002,.T.);
#1343=ORIENTED_EDGE('',*,*,#1003,.T.);
#1344=ORIENTED_EDGE('',*,*,#1004,.T.);
#1345=ORIENTED_EDGE('',*,*,#1005,.T.);
#1346=ORIENTED_EDGE('',*,*,#1006,.T.);
#1347=ORIENTED_EDGE('',*,*,#1000,.F.);
#1348=ORIENTED_EDGE('',*,*,#999,.F.);
#1349=ORIENTED_EDGE('',*,*,#1007,.T.);
#1350=ORIENTED_EDGE('',*,*,#1008,.F.);
#1351=ORIENTED_EDGE('',*,*,#979,.F.);
#1352=ORIENTED_EDGE('',*,*,#1009,.F.);
#1353=ORIENTED_EDGE('',*,*,#1001,.F.);
#1354=ORIENTED_EDGE('',*,*,#1009,.T.);
#1355=ORIENTED_EDGE('',*,*,#975,.F.);
#1356=ORIENTED_EDGE('',*,*,#1010,.F.);
#1357=ORIENTED_EDGE('',*,*,#1002,.F.);
#1358=ORIENTED_EDGE('',*,*,#1008,.T.);
#1359=ORIENTED_EDGE('',*,*,#1006,.F.);
#1360=ORIENTED_EDGE('',*,*,#1011,.F.);
#1361=ORIENTED_EDGE('',*,*,#983,.F.);
#1362=ORIENTED_EDGE('',*,*,#1010,.T.);
#1363=ORIENTED_EDGE('',*,*,#971,.F.);
#1364=ORIENTED_EDGE('',*,*,#1012,.F.);
#1365=ORIENTED_EDGE('',*,*,#1003,.F.);
#1366=ORIENTED_EDGE('',*,*,#1011,.T.);
#1367=ORIENTED_EDGE('',*,*,#1005,.F.);
#1368=ORIENTED_EDGE('',*,*,#1013,.F.);
#1369=ORIENTED_EDGE('',*,*,#987,.F.);
#1370=ORIENTED_EDGE('',*,*,#1012,.T.);
#1371=ORIENTED_EDGE('',*,*,#967,.F.);
#1372=ORIENTED_EDGE('',*,*,#1013,.T.);
#1373=ORIENTED_EDGE('',*,*,#1004,.F.);
#1374=ORIENTED_EDGE('',*,*,#1014,.T.);
#1375=ORIENTED_EDGE('',*,*,#1015,.T.);
#1376=ORIENTED_EDGE('',*,*,#1016,.T.);
#1377=ORIENTED_EDGE('',*,*,#1015,.F.);
#1378=ORIENTED_EDGE('',*,*,#1017,.T.);
#1379=ORIENTED_EDGE('',*,*,#1007,.F.);
#1380=ORIENTED_EDGE('',*,*,#1018,.T.);
#1381=ORIENTED_EDGE('',*,*,#1014,.F.);
#1382=ORIENTED_EDGE('',*,*,#1018,.F.);
#1383=ORIENTED_EDGE('',*,*,#1016,.F.);
#1384=ORIENTED_EDGE('',*,*,#1019,.T.);
#1385=ORIENTED_EDGE('',*,*,#1017,.F.);
#1386=ORIENTED_EDGE('',*,*,#1019,.F.);
#1387=ORIENTED_EDGE('',*,*,#1020,.T.);
#1388=ORIENTED_EDGE('',*,*,#1021,.T.);
#1389=ORIENTED_EDGE('',*,*,#1022,.F.);
#1390=ORIENTED_EDGE('',*,*,#1023,.T.);
#1391=ORIENTED_EDGE('',*,*,#1024,.T.);
#1392=ORIENTED_EDGE('',*,*,#1022,.T.);
#1393=ORIENTED_EDGE('',*,*,#1025,.T.);
#1394=ORIENTED_EDGE('',*,*,#1026,.F.);
#1395=ORIENTED_EDGE('',*,*,#1027,.T.);
#1396=ORIENTED_EDGE('',*,*,#1028,.T.);
#1397=ORIENTED_EDGE('',*,*,#1026,.T.);
#1398=ORIENTED_EDGE('',*,*,#1029,.T.);
#1399=ORIENTED_EDGE('',*,*,#1030,.F.);
#1400=ORIENTED_EDGE('',*,*,#1031,.T.);
#1401=ORIENTED_EDGE('',*,*,#1032,.T.);
#1402=ORIENTED_EDGE('',*,*,#1030,.T.);
#1403=ORIENTED_EDGE('',*,*,#1033,.T.);
#1404=ORIENTED_EDGE('',*,*,#1034,.F.);
#1405=ORIENTED_EDGE('',*,*,#1035,.T.);
#1406=ORIENTED_EDGE('',*,*,#1036,.T.);
#1407=ORIENTED_EDGE('',*,*,#1034,.T.);
#1408=ORIENTED_EDGE('',*,*,#1037,.T.);
#1409=ORIENTED_EDGE('',*,*,#1038,.F.);
#1410=ORIENTED_EDGE('',*,*,#1039,.T.);
#1411=ORIENTED_EDGE('',*,*,#1040,.T.);
#1412=ORIENTED_EDGE('',*,*,#1038,.T.);
#1413=ORIENTED_EDGE('',*,*,#1041,.T.);
#1414=ORIENTED_EDGE('',*,*,#1020,.F.);
#1415=ORIENTED_EDGE('',*,*,#1042,.T.);
#1416=ORIENTED_EDGE('',*,*,#1043,.T.);
#1417=ORIENTED_EDGE('',*,*,#1044,.T.);
#1418=ORIENTED_EDGE('',*,*,#1045,.T.);
#1419=ORIENTED_EDGE('',*,*,#1046,.T.);
#1420=ORIENTED_EDGE('',*,*,#1047,.T.);
#1421=ORIENTED_EDGE('',*,*,#1048,.T.);
#1422=ORIENTED_EDGE('',*,*,#1049,.T.);
#1423=ORIENTED_EDGE('',*,*,#1050,.T.);
#1424=ORIENTED_EDGE('',*,*,#1051,.T.);
#1425=ORIENTED_EDGE('',*,*,#1052,.T.);
#1426=ORIENTED_EDGE('',*,*,#1053,.T.);
#1427=ORIENTED_EDGE('',*,*,#1052,.F.);
#1428=ORIENTED_EDGE('',*,*,#1054,.T.);
#1429=ORIENTED_EDGE('',*,*,#1055,.F.);
#1430=ORIENTED_EDGE('',*,*,#1056,.T.);
#1431=ORIENTED_EDGE('',*,*,#1043,.F.);
#1432=ORIENTED_EDGE('',*,*,#1044,.F.);
#1433=ORIENTED_EDGE('',*,*,#1039,.F.);
#1434=ORIENTED_EDGE('',*,*,#1045,.F.);
#1435=ORIENTED_EDGE('',*,*,#1042,.F.);
#1436=ORIENTED_EDGE('',*,*,#1024,.F.);
#1437=ORIENTED_EDGE('',*,*,#1040,.F.);
#1438=ORIENTED_EDGE('',*,*,#1049,.F.);
#1439=ORIENTED_EDGE('',*,*,#1035,.F.);
#1440=ORIENTED_EDGE('',*,*,#1036,.F.);
#1441=ORIENTED_EDGE('',*,*,#1048,.F.);
#1442=ORIENTED_EDGE('',*,*,#1031,.F.);
#1443=ORIENTED_EDGE('',*,*,#1047,.F.);
#1444=ORIENTED_EDGE('',*,*,#1027,.F.);
#1445=ORIENTED_EDGE('',*,*,#1032,.F.);
#1446=ORIENTED_EDGE('',*,*,#1046,.F.);
#1447=ORIENTED_EDGE('',*,*,#1023,.F.);
#1448=ORIENTED_EDGE('',*,*,#1028,.F.);
#1449=ORIENTED_EDGE('',*,*,#1057,.T.);
#1450=ORIENTED_EDGE('',*,*,#1058,.T.);
#1451=ORIENTED_EDGE('',*,*,#1059,.T.);
#1452=ORIENTED_EDGE('',*,*,#1060,.T.);
#1453=ORIENTED_EDGE('',*,*,#1061,.T.);
#1454=ORIENTED_EDGE('',*,*,#1062,.T.);
#1455=ORIENTED_EDGE('',*,*,#1063,.T.);
#1456=ORIENTED_EDGE('',*,*,#1064,.T.);
#1457=ORIENTED_EDGE('',*,*,#1058,.F.);
#1458=ORIENTED_EDGE('',*,*,#1065,.T.);
#1459=ORIENTED_EDGE('',*,*,#1057,.F.);
#1460=ORIENTED_EDGE('',*,*,#1066,.T.);
#1461=ORIENTED_EDGE('',*,*,#1055,.T.);
#1462=ORIENTED_EDGE('',*,*,#1066,.F.);
#1463=ORIENTED_EDGE('',*,*,#1065,.F.);
#1464=ORIENTED_EDGE('',*,*,#1067,.F.);
#1465=ORIENTED_EDGE('',*,*,#1060,.F.);
#1466=ORIENTED_EDGE('',*,*,#1068,.F.);
#1467=ORIENTED_EDGE('',*,*,#1033,.F.);
#1468=ORIENTED_EDGE('',*,*,#1068,.T.);
#1469=ORIENTED_EDGE('',*,*,#1059,.F.);
#1470=ORIENTED_EDGE('',*,*,#1069,.F.);
#1471=ORIENTED_EDGE('',*,*,#1037,.F.);
#1472=ORIENTED_EDGE('',*,*,#1067,.T.);
#1473=ORIENTED_EDGE('',*,*,#1029,.F.);
#1474=ORIENTED_EDGE('',*,*,#1070,.F.);
#1475=ORIENTED_EDGE('',*,*,#1061,.F.);
#1476=ORIENTED_EDGE('',*,*,#1069,.T.);
#1477=ORIENTED_EDGE('',*,*,#1064,.F.);
#1478=ORIENTED_EDGE('',*,*,#1071,.F.);
#1479=ORIENTED_EDGE('',*,*,#1041,.F.);
#1480=ORIENTED_EDGE('',*,*,#1070,.T.);
#1481=ORIENTED_EDGE('',*,*,#1025,.F.);
#1482=ORIENTED_EDGE('',*,*,#1072,.F.);
#1483=ORIENTED_EDGE('',*,*,#1062,.F.);
#1484=ORIENTED_EDGE('',*,*,#1071,.T.);
#1485=ORIENTED_EDGE('',*,*,#1063,.F.);
#1486=ORIENTED_EDGE('',*,*,#1072,.T.);
#1487=ORIENTED_EDGE('',*,*,#1021,.F.);
#1488=ORIENTED_EDGE('',*,*,#1053,.F.);
#1489=ORIENTED_EDGE('',*,*,#1073,.T.);
#1490=ORIENTED_EDGE('',*,*,#1056,.F.);
#1491=ORIENTED_EDGE('',*,*,#1073,.F.);
#1492=ORIENTED_EDGE('',*,*,#1051,.F.);
#1493=ORIENTED_EDGE('',*,*,#1074,.T.);
#1494=ORIENTED_EDGE('',*,*,#1050,.F.);
#1495=ORIENTED_EDGE('',*,*,#1074,.F.);
#1496=ORIENTED_EDGE('',*,*,#1054,.F.);
#1497=ORIENTED_EDGE('',*,*,#1075,.F.);
#1498=ORIENTED_EDGE('',*,*,#1076,.F.);
#1499=ORIENTED_EDGE('',*,*,#1077,.F.);
#1500=ORIENTED_EDGE('',*,*,#1078,.T.);
#1501=ORIENTED_EDGE('',*,*,#1079,.T.);
#1502=ORIENTED_EDGE('',*,*,#1080,.F.);
#1503=ORIENTED_EDGE('',*,*,#1081,.T.);
#1504=ORIENTED_EDGE('',*,*,#1078,.F.);
#1505=ORIENTED_EDGE('',*,*,#1082,.F.);
#1506=ORIENTED_EDGE('',*,*,#1083,.T.);
#1507=ORIENTED_EDGE('',*,*,#1084,.T.);
#1508=ORIENTED_EDGE('',*,*,#1085,.F.);
#1509=ORIENTED_EDGE('',*,*,#1082,.T.);
#1510=ORIENTED_EDGE('',*,*,#1086,.F.);
#1511=ORIENTED_EDGE('',*,*,#1087,.T.);
#1512=ORIENTED_EDGE('',*,*,#1088,.F.);
#1513=ORIENTED_EDGE('',*,*,#1075,.T.);
#1514=ORIENTED_EDGE('',*,*,#1077,.T.);
#1515=ORIENTED_EDGE('',*,*,#1089,.F.);
#1516=ORIENTED_EDGE('',*,*,#1090,.F.);
#1517=ORIENTED_EDGE('',*,*,#1089,.T.);
#1518=ORIENTED_EDGE('',*,*,#1076,.T.);
#1519=ORIENTED_EDGE('',*,*,#1088,.T.);
#1520=ORIENTED_EDGE('',*,*,#1091,.T.);
#1521=ORIENTED_EDGE('',*,*,#1092,.T.);
#1522=ORIENTED_EDGE('',*,*,#1093,.T.);
#1523=ORIENTED_EDGE('',*,*,#1094,.F.);
#1524=ORIENTED_EDGE('',*,*,#1095,.F.);
#1525=ORIENTED_EDGE('',*,*,#1096,.F.);
#1526=ORIENTED_EDGE('',*,*,#1097,.T.);
#1527=ORIENTED_EDGE('',*,*,#1098,.T.);
#1528=ORIENTED_EDGE('',*,*,#1099,.T.);
#1529=ORIENTED_EDGE('',*,*,#1100,.F.);
#1530=ORIENTED_EDGE('',*,*,#1101,.T.);
#1531=ORIENTED_EDGE('',*,*,#1099,.F.);
#1532=ORIENTED_EDGE('',*,*,#1102,.T.);
#1533=ORIENTED_EDGE('',*,*,#1103,.F.);
#1534=ORIENTED_EDGE('',*,*,#1104,.T.);
#1535=ORIENTED_EDGE('',*,*,#1079,.F.);
#1536=ORIENTED_EDGE('',*,*,#1081,.F.);
#1537=ORIENTED_EDGE('',*,*,#1105,.T.);
#1538=ORIENTED_EDGE('',*,*,#1106,.F.);
#1539=ORIENTED_EDGE('',*,*,#1107,.F.);
#1540=ORIENTED_EDGE('',*,*,#1108,.F.);
#1541=ORIENTED_EDGE('',*,*,#1109,.F.);
#1542=ORIENTED_EDGE('',*,*,#1110,.F.);
#1543=ORIENTED_EDGE('',*,*,#1111,.F.);
#1544=ORIENTED_EDGE('',*,*,#1112,.T.);
#1545=ORIENTED_EDGE('',*,*,#1096,.T.);
#1546=ORIENTED_EDGE('',*,*,#1113,.T.);
#1547=ORIENTED_EDGE('',*,*,#1114,.T.);
#1548=ORIENTED_EDGE('',*,*,#1115,.T.);
#1549=ORIENTED_EDGE('',*,*,#1105,.F.);
#1550=ORIENTED_EDGE('',*,*,#1080,.T.);
#1551=ORIENTED_EDGE('',*,*,#1104,.F.);
#1552=ORIENTED_EDGE('',*,*,#1116,.T.);
#1553=ORIENTED_EDGE('',*,*,#1117,.F.);
#1554=ORIENTED_EDGE('',*,*,#1114,.F.);
#1555=ORIENTED_EDGE('',*,*,#1118,.F.);
#1556=ORIENTED_EDGE('',*,*,#1119,.T.);
#1557=ORIENTED_EDGE('',*,*,#1120,.F.);
#1558=ORIENTED_EDGE('',*,*,#1119,.F.);
#1559=ORIENTED_EDGE('',*,*,#1121,.F.);
#1560=ORIENTED_EDGE('',*,*,#1110,.T.);
#1561=ORIENTED_EDGE('',*,*,#1122,.F.);
#1562=ORIENTED_EDGE('',*,*,#1107,.T.);
#1563=ORIENTED_EDGE('',*,*,#1123,.T.);
#1564=ORIENTED_EDGE('',*,*,#1124,.F.);
#1565=ORIENTED_EDGE('',*,*,#1125,.F.);
#1566=ORIENTED_EDGE('',*,*,#1093,.F.);
#1567=ORIENTED_EDGE('',*,*,#1126,.T.);
#1568=ORIENTED_EDGE('',*,*,#1127,.F.);
#1569=ORIENTED_EDGE('',*,*,#1123,.F.);
#1570=ORIENTED_EDGE('',*,*,#1092,.F.);
#1571=ORIENTED_EDGE('',*,*,#1100,.T.);
#1572=ORIENTED_EDGE('',*,*,#1115,.F.);
#1573=ORIENTED_EDGE('',*,*,#1117,.T.);
#1574=ORIENTED_EDGE('',*,*,#1120,.T.);
#1575=ORIENTED_EDGE('',*,*,#1106,.T.);
#1576=ORIENTED_EDGE('',*,*,#1128,.T.);
#1577=ORIENTED_EDGE('',*,*,#1129,.F.);
#1578=ORIENTED_EDGE('',*,*,#1130,.F.);
#1579=ORIENTED_EDGE('',*,*,#1126,.F.);
#1580=ORIENTED_EDGE('',*,*,#1091,.F.);
#1581=ORIENTED_EDGE('',*,*,#1087,.F.);
#1582=ORIENTED_EDGE('',*,*,#1131,.T.);
#1583=ORIENTED_EDGE('',*,*,#1101,.F.);
#1584=ORIENTED_EDGE('',*,*,#1131,.F.);
#1585=ORIENTED_EDGE('',*,*,#1086,.T.);
#1586=ORIENTED_EDGE('',*,*,#1083,.F.);
#1587=ORIENTED_EDGE('',*,*,#1085,.T.);
#1588=ORIENTED_EDGE('',*,*,#1132,.T.);
#1589=ORIENTED_EDGE('',*,*,#1102,.F.);
#1590=ORIENTED_EDGE('',*,*,#1098,.F.);
#1591=ORIENTED_EDGE('',*,*,#1133,.T.);
#1592=ORIENTED_EDGE('',*,*,#1134,.T.);
#1593=ORIENTED_EDGE('',*,*,#1135,.F.);
#1594=ORIENTED_EDGE('',*,*,#1136,.T.);
#1595=ORIENTED_EDGE('',*,*,#1128,.F.);
#1596=ORIENTED_EDGE('',*,*,#1113,.F.);
#1597=ORIENTED_EDGE('',*,*,#1097,.F.);
#1598=ORIENTED_EDGE('',*,*,#1112,.F.);
#1599=ORIENTED_EDGE('',*,*,#1137,.F.);
#1600=ORIENTED_EDGE('',*,*,#1138,.F.);
#1601=ORIENTED_EDGE('',*,*,#1133,.F.);
#1602=ORIENTED_EDGE('',*,*,#1111,.T.);
#1603=ORIENTED_EDGE('',*,*,#1121,.T.);
#1604=ORIENTED_EDGE('',*,*,#1118,.T.);
#1605=ORIENTED_EDGE('',*,*,#1116,.F.);
#1606=ORIENTED_EDGE('',*,*,#1103,.T.);
#1607=ORIENTED_EDGE('',*,*,#1132,.F.);
#1608=ORIENTED_EDGE('',*,*,#1084,.F.);
#1609=ORIENTED_EDGE('',*,*,#1139,.F.);
#1610=ORIENTED_EDGE('',*,*,#1094,.T.);
#1611=ORIENTED_EDGE('',*,*,#1125,.T.);
#1612=ORIENTED_EDGE('',*,*,#1140,.F.);
#1613=ORIENTED_EDGE('',*,*,#1141,.F.);
#1614=ORIENTED_EDGE('',*,*,#1142,.F.);
#1615=ORIENTED_EDGE('',*,*,#1109,.T.);
#1616=ORIENTED_EDGE('',*,*,#1143,.T.);
#1617=ORIENTED_EDGE('',*,*,#1144,.F.);
#1618=ORIENTED_EDGE('',*,*,#1145,.F.);
#1619=ORIENTED_EDGE('',*,*,#1146,.F.);
#1620=ORIENTED_EDGE('',*,*,#1143,.F.);
#1621=ORIENTED_EDGE('',*,*,#1108,.T.);
#1622=ORIENTED_EDGE('',*,*,#1122,.T.);
#1623=ORIENTED_EDGE('',*,*,#1135,.T.);
#1624=ORIENTED_EDGE('',*,*,#1147,.T.);
#1625=ORIENTED_EDGE('',*,*,#1148,.T.);
#1626=ORIENTED_EDGE('',*,*,#1144,.T.);
#1627=ORIENTED_EDGE('',*,*,#1146,.T.);
#1628=ORIENTED_EDGE('',*,*,#1149,.T.);
#1629=ORIENTED_EDGE('',*,*,#1129,.T.);
#1630=ORIENTED_EDGE('',*,*,#1136,.F.);
#1631=ORIENTED_EDGE('',*,*,#1147,.F.);
#1632=ORIENTED_EDGE('',*,*,#1134,.F.);
#1633=ORIENTED_EDGE('',*,*,#1138,.T.);
#1634=ORIENTED_EDGE('',*,*,#1150,.F.);
#1635=ORIENTED_EDGE('',*,*,#1140,.T.);
#1636=ORIENTED_EDGE('',*,*,#1124,.T.);
#1637=ORIENTED_EDGE('',*,*,#1127,.T.);
#1638=ORIENTED_EDGE('',*,*,#1130,.T.);
#1639=ORIENTED_EDGE('',*,*,#1149,.F.);
#1640=ORIENTED_EDGE('',*,*,#1145,.T.);
#1641=ORIENTED_EDGE('',*,*,#1148,.F.);
#1642=ORIENTED_EDGE('',*,*,#1151,.F.);
#1643=ORIENTED_EDGE('',*,*,#1151,.T.);
#1644=ORIENTED_EDGE('',*,*,#1150,.T.);
#1645=ORIENTED_EDGE('',*,*,#1137,.T.);
#1646=ORIENTED_EDGE('',*,*,#1152,.T.);
#1647=ORIENTED_EDGE('',*,*,#1141,.T.);
#1648=ORIENTED_EDGE('',*,*,#1142,.T.);
#1649=ORIENTED_EDGE('',*,*,#1152,.F.);
#1650=ORIENTED_EDGE('',*,*,#1139,.T.);
#1651=ORIENTED_EDGE('',*,*,#1090,.T.);
#1652=ORIENTED_EDGE('',*,*,#1095,.T.);
#1653=CYLINDRICAL_SURFACE('',#1858,0.0254);
#1654=CYLINDRICAL_SURFACE('',#1861,0.0254);
#1655=CYLINDRICAL_SURFACE('',#1864,0.0381);
#1656=CYLINDRICAL_SURFACE('',#1869,0.00762);
#1657=CYLINDRICAL_SURFACE('',#1875,0.00762);
#1658=CYLINDRICAL_SURFACE('',#1900,0.01);
#1659=CYLINDRICAL_SURFACE('',#1902,0.0100000000000001);
#1660=CYLINDRICAL_SURFACE('',#1904,0.0100000000000001);
#1661=CYLINDRICAL_SURFACE('',#1906,0.0045);
#1662=CYLINDRICAL_SURFACE('',#1907,0.0045);
#1663=CYLINDRICAL_SURFACE('',#1908,0.0045);
#1664=CYLINDRICAL_SURFACE('',#1909,0.0045);
#1665=CYLINDRICAL_SURFACE('',#1910,0.01);
#1666=CYLINDRICAL_SURFACE('',#1943,0.003);
#1667=CYLINDRICAL_SURFACE('',#1966,0.0024585);
#1668=CYLINDRICAL_SURFACE('',#1987,0.00762);
#1669=CYLINDRICAL_SURFACE('',#1992,0.0277785949688766);
#1670=CYLINDRICAL_SURFACE('',#2001,0.0227670677706907);
#1671=CYLINDRICAL_SURFACE('',#2004,0.0227670677706907);
#1672=CYLINDRICAL_SURFACE('',#2008,0.02032);
#1673=CYLINDRICAL_SURFACE('',#2017,0.01508125);
#1674=CYLINDRICAL_SURFACE('',#2018,0.01508125);
#1675=CYLINDRICAL_SURFACE('',#2027,0.00762);
#1676=CYLINDRICAL_SURFACE('',#2030,0.0277785949688767);
#1677=CYLINDRICAL_SURFACE('',#2033,0.0331133532215094);
#1678=CYLINDRICAL_SURFACE('',#2035,0.0331133532215094);
#1679=ADVANCED_FACE('',(#273),#1653,.F.);
#1680=ADVANCED_FACE('',(#274),#1654,.F.);
#1681=ADVANCED_FACE('',(#275),#1655,.T.);
#1682=ADVANCED_FACE('',(#276,#210),#227,.T.);
#1683=ADVANCED_FACE('',(#277,#211),#228,.F.);
#1684=ADVANCED_FACE('',(#278),#1656,.F.);
#1685=ADVANCED_FACE('',(#279,#212),#229,.T.);
#1686=ADVANCED_FACE('',(#280,#213),#230,.F.);
#1687=ADVANCED_FACE('',(#281),#1657,.T.);
#1688=ADVANCED_FACE('',(#282),#231,.T.);
#1689=ADVANCED_FACE('',(#283),#232,.F.);
#1690=ADVANCED_FACE('',(#284,#214,#215,#216,#217,#218),#233,.T.);
#1691=ADVANCED_FACE('',(#285,#219,#220,#221,#222,#223),#234,.F.);
#1692=ADVANCED_FACE('',(#286),#235,.F.);
#1693=ADVANCED_FACE('',(#287),#1658,.T.);
#1694=ADVANCED_FACE('',(#288),#236,.F.);
#1695=ADVANCED_FACE('',(#289),#1659,.T.);
#1696=ADVANCED_FACE('',(#290),#237,.T.);
#1697=ADVANCED_FACE('',(#291),#1660,.T.);
#1698=ADVANCED_FACE('',(#292),#238,.T.);
#1699=ADVANCED_FACE('',(#293),#1661,.F.);
#1700=ADVANCED_FACE('',(#294),#1662,.F.);
#1701=ADVANCED_FACE('',(#295),#1663,.F.);
#1702=ADVANCED_FACE('',(#296),#1664,.F.);
#1703=ADVANCED_FACE('',(#297),#1665,.T.);
#1704=ADVANCED_FACE('',(#298),#239,.T.);
#1705=ADVANCED_FACE('',(#299),#240,.F.);
#1706=ADVANCED_FACE('',(#300),#241,.F.);
#1707=ADVANCED_FACE('',(#301),#242,.T.);
#1708=ADVANCED_FACE('',(#302),#243,.T.);
#1709=ADVANCED_FACE('',(#303),#244,.T.);
#1710=ADVANCED_FACE('',(#304),#245,.T.);
#1711=ADVANCED_FACE('',(#305),#246,.T.);
#1712=ADVANCED_FACE('',(#306),#247,.T.);
#1713=ADVANCED_FACE('',(#307),#248,.T.);
#1714=ADVANCED_FACE('',(#308),#93,.T.);
#1715=ADVANCED_FACE('',(#309),#94,.T.);
#1716=ADVANCED_FACE('',(#310),#95,.T.);
#1717=ADVANCED_FACE('',(#311),#96,.T.);
#1718=ADVANCED_FACE('',(#312),#97,.T.);
#1719=ADVANCED_FACE('',(#313),#98,.T.);
#1720=ADVANCED_FACE('',(#314),#249,.T.);
#1721=ADVANCED_FACE('',(#315),#90,.T.);
#1722=ADVANCED_FACE('',(#316),#99,.T.);
#1723=ADVANCED_FACE('',(#317,#224),#250,.F.);
#1724=ADVANCED_FACE('',(#318),#78,.F.);
#1725=ADVANCED_FACE('',(#319),#79,.F.);
#1726=ADVANCED_FACE('',(#320),#80,.F.);
#1727=ADVANCED_FACE('',(#321),#81,.F.);
#1728=ADVANCED_FACE('',(#322),#82,.F.);
#1729=ADVANCED_FACE('',(#323),#83,.F.);
#1730=ADVANCED_FACE('',(#324),#1666,.T.);
#1731=ADVANCED_FACE('',(#325),#251,.T.);
#1732=ADVANCED_FACE('',(#326),#91,.F.);
#1733=ADVANCED_FACE('',(#327),#100,.T.);
#1734=ADVANCED_FACE('',(#328),#252,.T.);
#1735=ADVANCED_FACE('',(#329),#253,.T.);
#1736=ADVANCED_FACE('',(#330),#254,.T.);
#1737=ADVANCED_FACE('',(#331),#255,.T.);
#1738=ADVANCED_FACE('',(#332),#256,.T.);
#1739=ADVANCED_FACE('',(#333),#257,.T.);
#1740=ADVANCED_FACE('',(#334,#225),#258,.T.);
#1741=ADVANCED_FACE('',(#335),#1667,.F.);
#1742=ADVANCED_FACE('',(#336,#226),#259,.F.);
#1743=ADVANCED_FACE('',(#337),#101,.T.);
#1744=ADVANCED_FACE('',(#338),#102,.T.);
#1745=ADVANCED_FACE('',(#339),#103,.T.);
#1746=ADVANCED_FACE('',(#340),#104,.T.);
#1747=ADVANCED_FACE('',(#341),#105,.T.);
#1748=ADVANCED_FACE('',(#342),#106,.T.);
#1749=ADVANCED_FACE('',(#343),#107,.T.);
#1750=ADVANCED_FACE('',(#344),#92,.T.);
#1751=ADVANCED_FACE('',(#345),#84,.F.);
#1752=ADVANCED_FACE('',(#346),#85,.F.);
#1753=ADVANCED_FACE('',(#347),#86,.F.);
#1754=ADVANCED_FACE('',(#348),#87,.F.);
#1755=ADVANCED_FACE('',(#349),#88,.F.);
#1756=ADVANCED_FACE('',(#350),#89,.F.);
#1757=ADVANCED_FACE('',(#351),#108,.F.);
#1758=ADVANCED_FACE('',(#352),#109,.F.);
#1759=ADVANCED_FACE('',(#353),#1668,.F.);
#1760=ADVANCED_FACE('',(#354),#260,.F.);
#1761=ADVANCED_FACE('',(#355),#1669,.T.);
#1762=ADVANCED_FACE('',(#356),#261,.T.);
#1763=ADVANCED_FACE('',(#357),#262,.F.);
#1764=ADVANCED_FACE('',(#358),#263,.F.);
#1765=ADVANCED_FACE('',(#359),#1670,.F.);
#1766=ADVANCED_FACE('',(#360),#1671,.F.);
#1767=ADVANCED_FACE('',(#361),#264,.T.);
#1768=ADVANCED_FACE('',(#362),#1672,.F.);
#1769=ADVANCED_FACE('',(#363),#265,.F.);
#1770=ADVANCED_FACE('',(#364),#266,.T.);
#1771=ADVANCED_FACE('',(#365),#267,.T.);
#1772=ADVANCED_FACE('',(#366),#268,.T.);
#1773=ADVANCED_FACE('',(#367),#1673,.T.);
#1774=ADVANCED_FACE('',(#368),#1674,.T.);
#1775=ADVANCED_FACE('',(#369),#269,.T.);
#1776=ADVANCED_FACE('',(#370),#270,.F.);
#1777=ADVANCED_FACE('',(#371),#1675,.F.);
#1778=ADVANCED_FACE('',(#372),#271,.F.);
#1779=ADVANCED_FACE('',(#373),#1676,.T.);
#1780=ADVANCED_FACE('',(#374),#272,.T.);
#1781=ADVANCED_FACE('',(#375),#1677,.T.);
#1782=ADVANCED_FACE('',(#376),#1678,.T.);
#1783=CLOSED_SHELL('',(#1679,#1680,#1681,#1682,#1683,#1684,#1685,#1686));
#1784=CLOSED_SHELL('',(#1687,#1688,#1689));
#1785=CLOSED_SHELL('',(#1690,#1691,#1692,#1693,#1694,#1695,#1696,#1697,
#1698,#1699,#1700,#1701,#1702,#1703,#1704,#1705,#1706,#1707));
#1786=CLOSED_SHELL('',(#1708,#1709,#1710,#1711,#1712,#1713,#1714,#1715,
#1716,#1717,#1718,#1719,#1720,#1721,#1722,#1723,#1724,#1725,#1726,#1727,
#1728,#1729,#1730,#1731,#1732,#1733));
#1787=CLOSED_SHELL('',(#1734,#1735,#1736,#1737,#1738,#1739,#1740,#1741,
#1742,#1743,#1744,#1745,#1746,#1747,#1748,#1749,#1750,#1751,#1752,#1753,
#1754,#1755,#1756,#1757,#1758));
#1788=CLOSED_SHELL('',(#1759,#1760,#1761,#1762,#1763,#1764,#1765,#1766,
#1767,#1768,#1769,#1770,#1771,#1772,#1773,#1774,#1775,#1776,#1777,#1778,
#1779,#1780,#1781,#1782));
#1789=DERIVED_UNIT_ELEMENT(#1801,1.);
#1790=DERIVED_UNIT_ELEMENT(#3833,-3.);
#1791=DERIVED_UNIT_ELEMENT(#1801,1.);
#1792=DERIVED_UNIT_ELEMENT(#3833,-3.);
#1793=DERIVED_UNIT_ELEMENT(#1801,1.);
#1794=DERIVED_UNIT_ELEMENT(#3833,-3.);
#1795=DERIVED_UNIT_ELEMENT(#1801,1.);
#1796=DERIVED_UNIT_ELEMENT(#3833,-3.);
#1797=DERIVED_UNIT_ELEMENT(#1801,1.);
#1798=DERIVED_UNIT_ELEMENT(#3833,-3.);
#1799=DERIVED_UNIT_ELEMENT(#1801,1.);
#1800=DERIVED_UNIT_ELEMENT(#3833,-3.);
#1801=(
MASS_UNIT()
NAMED_UNIT(*)
SI_UNIT(.KILO.,.GRAM.)
);
#1802=DERIVED_UNIT((#1789,#1790));
#1803=DERIVED_UNIT((#1791,#1792));
#1804=DERIVED_UNIT((#1793,#1794));
#1805=DERIVED_UNIT((#1795,#1796));
#1806=DERIVED_UNIT((#1797,#1798));
#1807=DERIVED_UNIT((#1799,#1800));
#1808=MEASURE_REPRESENTATION_ITEM('density measure',
POSITIVE_RATIO_MEASURE(7850.),#1802);
#1809=MEASURE_REPRESENTATION_ITEM('density measure',
POSITIVE_RATIO_MEASURE(7850.),#1803);
#1810=MEASURE_REPRESENTATION_ITEM('density measure',
POSITIVE_RATIO_MEASURE(7850.),#1804);
#1811=MEASURE_REPRESENTATION_ITEM('density measure',
POSITIVE_RATIO_MEASURE(7850.),#1805);
#1812=MEASURE_REPRESENTATION_ITEM('density measure',
POSITIVE_RATIO_MEASURE(7850.),#1806);
#1813=MEASURE_REPRESENTATION_ITEM('density measure',
POSITIVE_RATIO_MEASURE(7850.),#1807);
#1814=PROPERTY_DEFINITION_REPRESENTATION(#1844,#1826);
#1815=PROPERTY_DEFINITION_REPRESENTATION(#1845,#1827);
#1816=PROPERTY_DEFINITION_REPRESENTATION(#1846,#1828);
#1817=PROPERTY_DEFINITION_REPRESENTATION(#1847,#1829);
#1818=PROPERTY_DEFINITION_REPRESENTATION(#1848,#1830);
#1819=PROPERTY_DEFINITION_REPRESENTATION(#1849,#1831);
#1820=PROPERTY_DEFINITION_REPRESENTATION(#1850,#1832);
#1821=PROPERTY_DEFINITION_REPRESENTATION(#1851,#1833);
#1822=PROPERTY_DEFINITION_REPRESENTATION(#1852,#1834);
#1823=PROPERTY_DEFINITION_REPRESENTATION(#1853,#1835);
#1824=PROPERTY_DEFINITION_REPRESENTATION(#1854,#1836);
#1825=PROPERTY_DEFINITION_REPRESENTATION(#1855,#1837);
#1826=REPRESENTATION('material name',(#1838),#3826);
#1827=REPRESENTATION('density',(#1808),#3826);
#1828=REPRESENTATION('material name',(#1839),#3827);
#1829=REPRESENTATION('density',(#1809),#3827);
#1830=REPRESENTATION('material name',(#1840),#3828);
#1831=REPRESENTATION('density',(#1810),#3828);
#1832=REPRESENTATION('material name',(#1841),#3829);
#1833=REPRESENTATION('density',(#1811),#3829);
#1834=REPRESENTATION('material name',(#1842),#3830);
#1835=REPRESENTATION('density',(#1812),#3830);
#1836=REPRESENTATION('material name',(#1843),#3831);
#1837=REPRESENTATION('density',(#1813),#3831);
#1838=DESCRIPTIVE_REPRESENTATION_ITEM('Steel','Steel');
#1839=DESCRIPTIVE_REPRESENTATION_ITEM('Steel','Steel');
#1840=DESCRIPTIVE_REPRESENTATION_ITEM('Steel','Steel');
#1841=DESCRIPTIVE_REPRESENTATION_ITEM('Steel','Steel');
#1842=DESCRIPTIVE_REPRESENTATION_ITEM('Steel','Steel');
#1843=DESCRIPTIVE_REPRESENTATION_ITEM('Steel','Steel');
#1844=PROPERTY_DEFINITION('material property','material name',#3871);
#1845=PROPERTY_DEFINITION('material property','density of part',#3871);
#1846=PROPERTY_DEFINITION('material property','material name',#3872);
#1847=PROPERTY_DEFINITION('material property','density of part',#3872);
#1848=PROPERTY_DEFINITION('material property','material name',#3873);
#1849=PROPERTY_DEFINITION('material property','density of part',#3873);
#1850=PROPERTY_DEFINITION('material property','material name',#3874);
#1851=PROPERTY_DEFINITION('material property','density of part',#3874);
#1852=PROPERTY_DEFINITION('material property','material name',#3875);
#1853=PROPERTY_DEFINITION('material property','density of part',#3875);
#1854=PROPERTY_DEFINITION('material property','material name',#3876);
#1855=PROPERTY_DEFINITION('material property','density of part',#3876);
#1856=AXIS2_PLACEMENT_3D('',#2525,#2048,#2049);
#1857=AXIS2_PLACEMENT_3D('',#2526,#2050,#2051);
#1858=AXIS2_PLACEMENT_3D('',#2527,#2052,#2053);
#1859=AXIS2_PLACEMENT_3D('',#2529,#2054,#2055);
#1860=AXIS2_PLACEMENT_3D('',#2532,#2057,#2058);
#1861=AXIS2_PLACEMENT_3D('',#2533,#2059,#2060);
#1862=AXIS2_PLACEMENT_3D('',#2535,#2061,#2062);
#1863=AXIS2_PLACEMENT_3D('',#2538,#2064,#2065);
#1864=AXIS2_PLACEMENT_3D('',#2539,#2066,#2067);
#1865=AXIS2_PLACEMENT_3D('',#2541,#2068,#2069);
#1866=AXIS2_PLACEMENT_3D('',#2544,#2071,#2072);
#1867=AXIS2_PLACEMENT_3D('',#2545,#2073,#2074);
#1868=AXIS2_PLACEMENT_3D('',#2546,#2075,#2076);
#1869=AXIS2_PLACEMENT_3D('',#2547,#2077,#2078);
#1870=AXIS2_PLACEMENT_3D('',#2549,#2079,#2080);
#1871=AXIS2_PLACEMENT_3D('',#2552,#2082,#2083);
#1872=AXIS2_PLACEMENT_3D('',#2553,#2084,#2085);
#1873=AXIS2_PLACEMENT_3D('',#2554,#2086,#2087);
#1874=AXIS2_PLACEMENT_3D('',#2555,#2088,#2089);
#1875=AXIS2_PLACEMENT_3D('',#2556,#2090,#2091);
#1876=AXIS2_PLACEMENT_3D('',#2558,#2092,#2093);
#1877=AXIS2_PLACEMENT_3D('',#2561,#2095,#2096);
#1878=AXIS2_PLACEMENT_3D('',#2562,#2097,#2098);
#1879=AXIS2_PLACEMENT_3D('',#2563,#2099,#2100);
#1880=AXIS2_PLACEMENT_3D('',#2564,#2101,#2102);
#1881=AXIS2_PLACEMENT_3D('',#2565,#2103,#2104);
#1882=AXIS2_PLACEMENT_3D('',#2570,#2106,#2107);
#1883=AXIS2_PLACEMENT_3D('',#2574,#2109,#2110);
#1884=AXIS2_PLACEMENT_3D('',#2578,#2112,#2113);
#1885=AXIS2_PLACEMENT_3D('',#2581,#2115,#2116);
#1886=AXIS2_PLACEMENT_3D('',#2591,#2121,#2122);
#1887=AXIS2_PLACEMENT_3D('',#2593,#2123,#2124);
#1888=AXIS2_PLACEMENT_3D('',#2595,#2125,#2126);
#1889=AXIS2_PLACEMENT_3D('',#2597,#2127,#2128);
#1890=AXIS2_PLACEMENT_3D('',#2598,#2129,#2130);
#1891=AXIS2_PLACEMENT_3D('',#2603,#2132,#2133);
#1892=AXIS2_PLACEMENT_3D('',#2607,#2135,#2136);
#1893=AXIS2_PLACEMENT_3D('',#2611,#2138,#2139);
#1894=AXIS2_PLACEMENT_3D('',#2614,#2141,#2142);
#1895=AXIS2_PLACEMENT_3D('',#2616,#2143,#2144);
#1896=AXIS2_PLACEMENT_3D('',#2618,#2145,#2146);
#1897=AXIS2_PLACEMENT_3D('',#2620,#2147,#2148);
#1898=AXIS2_PLACEMENT_3D('',#2622,#2149,#2150);
#1899=AXIS2_PLACEMENT_3D('',#2631,#2155,#2156);
#1900=AXIS2_PLACEMENT_3D('',#2634,#2159,#2160);
#1901=AXIS2_PLACEMENT_3D('',#2636,#2162,#2163);
#1902=AXIS2_PLACEMENT_3D('',#2638,#2165,#2166);
#1903=AXIS2_PLACEMENT_3D('',#2640,#2168,#2169);
#1904=AXIS2_PLACEMENT_3D('',#2642,#2171,#2172);
#1905=AXIS2_PLACEMENT_3D('',#2644,#2174,#2175);
#1906=AXIS2_PLACEMENT_3D('',#2646,#2177,#2178);
#1907=AXIS2_PLACEMENT_3D('',#2648,#2180,#2181);
#1908=AXIS2_PLACEMENT_3D('',#2650,#2183,#2184);
#1909=AXIS2_PLACEMENT_3D('',#2652,#2186,#2187);
#1910=AXIS2_PLACEMENT_3D('',#2654,#2189,#2190);
#1911=AXIS2_PLACEMENT_3D('',#2655,#2191,#2192);
#1912=AXIS2_PLACEMENT_3D('',#2658,#2195,#2196);
#1913=AXIS2_PLACEMENT_3D('',#2660,#2198,#2199);
#1914=AXIS2_PLACEMENT_3D('',#2662,#2201,#2202);
#1915=AXIS2_PLACEMENT_3D('',#2663,#2203,#2204);
#1916=AXIS2_PLACEMENT_3D('',#2664,#2205,#2206);
#1917=AXIS2_PLACEMENT_3D('',#2694,#2209,#2210);
#1918=AXIS2_PLACEMENT_3D('',#2721,#2212,#2213);
#1919=AXIS2_PLACEMENT_3D('',#2748,#2215,#2216);
#1920=AXIS2_PLACEMENT_3D('',#2775,#2218,#2219);
#1921=AXIS2_PLACEMENT_3D('',#2802,#2221,#2222);
#1922=AXIS2_PLACEMENT_3D('',#2826,#2223,#2224);
#1923=AXIS2_PLACEMENT_3D('',#2827,#2225,#2226);
#1924=AXIS2_PLACEMENT_3D('',#2828,#2227,#2228);
#1925=AXIS2_PLACEMENT_3D('',#2829,#2229,#2230);
#1926=AXIS2_PLACEMENT_3D('',#2830,#2231,#2232);
#1927=AXIS2_PLACEMENT_3D('',#2831,#2233,#2234);
#1928=AXIS2_PLACEMENT_3D('',#2832,#2235,#2236);
#1929=AXIS2_PLACEMENT_3D('',#2833,#2237,#2238);
#1930=AXIS2_PLACEMENT_3D('',#2834,#2239,#2240);
#1931=AXIS2_PLACEMENT_3D('',#2835,#2241,#2242);
#1932=AXIS2_PLACEMENT_3D('',#2836,#2243,#2244);
#1933=AXIS2_PLACEMENT_3D('',#2837,#2245,#2246);
#1934=AXIS2_PLACEMENT_3D('',#2838,#2247,#2248);
#1935=AXIS2_PLACEMENT_3D('',#2839,#2249,#2250);
#1936=AXIS2_PLACEMENT_3D('',#2842,#2251,#2252);
#1937=AXIS2_PLACEMENT_3D('',#2843,#2253,#2254);
#1938=AXIS2_PLACEMENT_3D('',#2845,#2255,#2256);
#1939=AXIS2_PLACEMENT_3D('',#2846,#2257,#2258);
#1940=AXIS2_PLACEMENT_3D('',#2847,#2259,#2260);
#1941=AXIS2_PLACEMENT_3D('',#2885,#2262,#2263);
#1942=AXIS2_PLACEMENT_3D('',#2887,#2264,#2265);
#1943=AXIS2_PLACEMENT_3D('',#3050,#2266,#2267);
#1944=AXIS2_PLACEMENT_3D('',#3052,#2268,#2269);
#1945=AXIS2_PLACEMENT_3D('',#3055,#2271,#2272);
#1946=AXIS2_PLACEMENT_3D('',#3056,#2273,#2274);
#1947=AXIS2_PLACEMENT_3D('',#3058,#2275,#2276);
#1948=AXIS2_PLACEMENT_3D('',#3059,#2277,#2278);
#1949=AXIS2_PLACEMENT_3D('',#3060,#2279,#2280);
#1950=AXIS2_PLACEMENT_3D('',#3061,#2281,#2282);
#1951=AXIS2_PLACEMENT_3D('',#3063,#2284,#2285);
#1952=AXIS2_PLACEMENT_3D('',#3064,#2286,#2287);
#1953=AXIS2_PLACEMENT_3D('',#3094,#2290,#2291);
#1954=AXIS2_PLACEMENT_3D('',#3121,#2293,#2294);
#1955=AXIS2_PLACEMENT_3D('',#3148,#2296,#2297);
#1956=AXIS2_PLACEMENT_3D('',#3175,#2299,#2300);
#1957=AXIS2_PLACEMENT_3D('',#3202,#2302,#2303);
#1958=AXIS2_PLACEMENT_3D('',#3226,#2304,#2305);
#1959=AXIS2_PLACEMENT_3D('',#3227,#2306,#2307);
#1960=AXIS2_PLACEMENT_3D('',#3228,#2308,#2309);
#1961=AXIS2_PLACEMENT_3D('',#3229,#2310,#2311);
#1962=AXIS2_PLACEMENT_3D('',#3230,#2312,#2313);
#1963=AXIS2_PLACEMENT_3D('',#3231,#2314,#2315);
#1964=AXIS2_PLACEMENT_3D('',#3232,#2316,#2317);
#1965=AXIS2_PLACEMENT_3D('',#3234,#2318,#2319);
#1966=AXIS2_PLACEMENT_3D('',#3235,#2320,#2321);
#1967=AXIS2_PLACEMENT_3D('',#3238,#2322,#2323);
#1968=AXIS2_PLACEMENT_3D('',#3241,#2325,#2326);
#1969=AXIS2_PLACEMENT_3D('',#3242,#2327,#2328);
#1970=AXIS2_PLACEMENT_3D('',#3243,#2329,#2330);
#1971=AXIS2_PLACEMENT_3D('',#3245,#2331,#2332);
#1972=AXIS2_PLACEMENT_3D('',#3247,#2333,#2334);
#1973=AXIS2_PLACEMENT_3D('',#3248,#2335,#2336);
#1974=AXIS2_PLACEMENT_3D('',#3249,#2337,#2338);
#1975=AXIS2_PLACEMENT_3D('',#3250,#2339,#2340);
#1976=AXIS2_PLACEMENT_3D('',#3251,#2341,#2342);
#1977=AXIS2_PLACEMENT_3D('',#3252,#2343,#2344);
#1978=AXIS2_PLACEMENT_3D('',#3253,#2345,#2346);
#1979=AXIS2_PLACEMENT_3D('',#3254,#2347,#2348);
#1980=AXIS2_PLACEMENT_3D('',#3257,#2349,#2350);
#1981=AXIS2_PLACEMENT_3D('',#3295,#2352,#2353);
#1982=AXIS2_PLACEMENT_3D('',#3296,#2354,#2355);
#1983=AXIS2_PLACEMENT_3D('',#3297,#2356,#2357);
#1984=AXIS2_PLACEMENT_3D('',#3460,#2358,#2359);
#1985=AXIS2_PLACEMENT_3D('',#3462,#2361,#2362);
#1986=AXIS2_PLACEMENT_3D('',#3464,#2364,#2365);
#1987=AXIS2_PLACEMENT_3D('',#3465,#2366,#2367);
#1988=AXIS2_PLACEMENT_3D('',#3483,#2368,#2369);
#1989=AXIS2_PLACEMENT_3D('',#3518,#2371,#2372);
#1990=AXIS2_PLACEMENT_3D('',#3535,#2373,#2374);
#1991=AXIS2_PLACEMENT_3D('',#3539,#2376,#2377);
#1992=AXIS2_PLACEMENT_3D('',#3540,#2378,#2379);
#1993=AXIS2_PLACEMENT_3D('',#3543,#2380,#2381);
#1994=AXIS2_PLACEMENT_3D('',#3567,#2382,#2383);
#1995=AXIS2_PLACEMENT_3D('',#3571,#2386,#2387);
#1996=AXIS2_PLACEMENT_3D('',#3572,#2388,#2389);
#1997=AXIS2_PLACEMENT_3D('',#3582,#2395,#2396);
#1998=AXIS2_PLACEMENT_3D('',#3586,#2398,#2399);
#1999=AXIS2_PLACEMENT_3D('',#3587,#2400,#2401);
#2000=AXIS2_PLACEMENT_3D('',#3590,#2402,#2403);
#2001=AXIS2_PLACEMENT_3D('',#3592,#2405,#2406);
#2002=AXIS2_PLACEMENT_3D('',#3595,#2407,#2408);
#2003=AXIS2_PLACEMENT_3D('',#3618,#2409,#2410);
#2004=AXIS2_PLACEMENT_3D('',#3621,#2413,#2414);
#2005=AXIS2_PLACEMENT_3D('',#3624,#2415,#2416);
#2006=AXIS2_PLACEMENT_3D('',#3664,#2419,#2420);
#2007=AXIS2_PLACEMENT_3D('',#3685,#2421,#2422);
#2008=AXIS2_PLACEMENT_3D('',#3691,#2426,#2427);
#2009=AXIS2_PLACEMENT_3D('',#3693,#2428,#2429);
#2010=AXIS2_PLACEMENT_3D('',#3695,#2430,#2431);
#2011=AXIS2_PLACEMENT_3D('',#3697,#2433,#2434);
#2012=AXIS2_PLACEMENT_3D('',#3700,#2437,#2438);
#2013=AXIS2_PLACEMENT_3D('',#3701,#2439,#2440);
#2014=AXIS2_PLACEMENT_3D('',#3707,#2444,#2445);
#2015=AXIS2_PLACEMENT_3D('',#3711,#2448,#2449);
#2016=AXIS2_PLACEMENT_3D('',#3715,#2451,#2452);
#2017=AXIS2_PLACEMENT_3D('',#3718,#2455,#2456);
#2018=AXIS2_PLACEMENT_3D('',#3720,#2458,#2459);
#2019=AXIS2_PLACEMENT_3D('',#3732,#2461,#2462);
#2020=AXIS2_PLACEMENT_3D('',#3747,#2463,#2464);
#2021=AXIS2_PLACEMENT_3D('',#3750,#2465,#2466);
#2022=AXIS2_PLACEMENT_3D('',#3751,#2467,#2468);
#2023=AXIS2_PLACEMENT_3D('',#3752,#2469,#2470);
#2024=AXIS2_PLACEMENT_3D('',#3753,#2471,#2472);
#2025=AXIS2_PLACEMENT_3D('',#3757,#2474,#2475);
#2026=AXIS2_PLACEMENT_3D('',#3758,#2476,#2477);
#2027=AXIS2_PLACEMENT_3D('',#3759,#2478,#2479);
#2028=AXIS2_PLACEMENT_3D('',#3778,#2481,#2482);
#2029=AXIS2_PLACEMENT_3D('',#3793,#2483,#2484);
#2030=AXIS2_PLACEMENT_3D('',#3795,#2486,#2487);
#2031=AXIS2_PLACEMENT_3D('',#3799,#2490,#2491);
#2032=AXIS2_PLACEMENT_3D('',#3800,#2492,#2493);
#2033=AXIS2_PLACEMENT_3D('',#3802,#2495,#2496);
#2034=AXIS2_PLACEMENT_3D('',#3803,#2497,#2498);
#2035=AXIS2_PLACEMENT_3D('',#3804,#2499,#2500);
#2036=AXIS2_PLACEMENT_3D('',#3805,#2501,#2502);
#2037=AXIS2_PLACEMENT_3D('',#3806,#2503,#2504);
#2038=AXIS2_PLACEMENT_3D('',#3807,#2505,#2506);
#2039=AXIS2_PLACEMENT_3D('',#3808,#2507,#2508);
#2040=AXIS2_PLACEMENT_3D('',#3809,#2509,#2510);
#2041=AXIS2_PLACEMENT_3D('',#3810,#2511,#2512);
#2042=AXIS2_PLACEMENT_3D('',#3811,#2513,#2514);
#2043=AXIS2_PLACEMENT_3D('',#3812,#2515,#2516);
#2044=AXIS2_PLACEMENT_3D('',#3813,#2517,#2518);
#2045=AXIS2_PLACEMENT_3D('',#3814,#2519,#2520);
#2046=AXIS2_PLACEMENT_3D('',#3815,#2521,#2522);
#2047=AXIS2_PLACEMENT_3D('',#3816,#2523,#2524);
#2048=DIRECTION('axis',(0.,0.,1.));
#2049=DIRECTION('refdir',(1.,0.,0.));
#2050=DIRECTION('axis',(0.,0.,1.));
#2051=DIRECTION('refdir',(1.,0.,0.));
#2052=DIRECTION('center_axis',(-1.,0.,0.));
#2053=DIRECTION('ref_axis',(0.,0.,1.));
#2054=DIRECTION('center_axis',(1.,0.,0.));
#2055=DIRECTION('ref_axis',(0.,0.,-1.));
#2056=DIRECTION('',(-1.,0.,0.));
#2057=DIRECTION('center_axis',(1.,0.,0.));
#2058=DIRECTION('ref_axis',(0.,0.,-1.));
#2059=DIRECTION('center_axis',(-1.,0.,0.));
#2060=DIRECTION('ref_axis',(0.,0.,1.));
#2061=DIRECTION('center_axis',(1.,0.,0.));
#2062=DIRECTION('ref_axis',(0.,0.,-1.));
#2063=DIRECTION('',(-1.,0.,0.));
#2064=DIRECTION('center_axis',(1.,0.,0.));
#2065=DIRECTION('ref_axis',(0.,0.,-1.));
#2066=DIRECTION('center_axis',(-1.,0.,0.));
#2067=DIRECTION('ref_axis',(0.,0.,1.));
#2068=DIRECTION('center_axis',(1.,0.,0.));
#2069=DIRECTION('ref_axis',(0.,0.,-1.));
#2070=DIRECTION('',(1.,0.,0.));
#2071=DIRECTION('center_axis',(1.,0.,0.));
#2072=DIRECTION('ref_axis',(0.,0.,-1.));
#2073=DIRECTION('center_axis',(1.,0.,0.));
#2074=DIRECTION('ref_axis',(0.,1.,0.));
#2075=DIRECTION('center_axis',(1.,0.,0.));
#2076=DIRECTION('ref_axis',(0.,1.,0.));
#2077=DIRECTION('center_axis',(-1.,0.,0.));
#2078=DIRECTION('ref_axis',(0.,0.,1.));
#2079=DIRECTION('center_axis',(1.,0.,0.));
#2080=DIRECTION('ref_axis',(0.,0.,-1.));
#2081=DIRECTION('',(-1.,0.,0.));
#2082=DIRECTION('center_axis',(1.,0.,0.));
#2083=DIRECTION('ref_axis',(0.,0.,-1.));
#2084=DIRECTION('center_axis',(1.,0.,0.));
#2085=DIRECTION('ref_axis',(0.,1.,0.));
#2086=DIRECTION('center_axis',(1.,0.,0.));
#2087=DIRECTION('ref_axis',(0.,1.,0.));
#2088=DIRECTION('axis',(0.,0.,1.));
#2089=DIRECTION('refdir',(1.,0.,0.));
#2090=DIRECTION('center_axis',(-1.,0.,0.));
#2091=DIRECTION('ref_axis',(0.,0.,1.));
#2092=DIRECTION('center_axis',(1.,0.,0.));
#2093=DIRECTION('ref_axis',(0.,0.,-1.));
#2094=DIRECTION('',(1.,0.,0.));
#2095=DIRECTION('center_axis',(1.,0.,0.));
#2096=DIRECTION('ref_axis',(0.,0.,-1.));
#2097=DIRECTION('center_axis',(1.,0.,0.));
#2098=DIRECTION('ref_axis',(0.,1.,0.));
#2099=DIRECTION('center_axis',(1.,0.,0.));
#2100=DIRECTION('ref_axis',(0.,1.,0.));
#2101=DIRECTION('axis',(0.,0.,1.));
#2102=DIRECTION('refdir',(1.,0.,0.));
#2103=DIRECTION('center_axis',(-4.62592926927149E-16,-2.83256473634769E-32,
-1.));
#2104=DIRECTION('ref_axis',(-1.,1.3103244120977E-47,4.62592926927149E-16));
#2105=DIRECTION('',(1.3103244120977E-47,-1.,2.83256473634769E-32));
#2106=DIRECTION('center_axis',(4.62592926927149E-16,2.83256473634769E-32,
1.));
#2107=DIRECTION('ref_axis',(1.,-7.59501135632552E-64,-4.62592926927149E-16));
#2108=DIRECTION('',(1.,-4.67973004320639E-49,-4.62592926927149E-16));
#2109=DIRECTION('center_axis',(4.62592926927149E-16,2.83256473634769E-32,
1.));
#2110=DIRECTION('ref_axis',(1.,-7.59501135632553E-64,-4.62592926927149E-16));
#2111=DIRECTION('',(1.3103244120977E-47,-1.,2.83256473634769E-32));
#2112=DIRECTION('center_axis',(4.62592926927149E-16,2.83256473634769E-32,
1.));
#2113=DIRECTION('ref_axis',(1.,-7.59501135632553E-64,-4.62592926927149E-16));
#2114=DIRECTION('',(1.,-4.67973004320639E-49,-4.62592926927149E-16));
#2115=DIRECTION('center_axis',(4.62592926927149E-16,2.83256473634769E-32,
1.));
#2116=DIRECTION('ref_axis',(1.,-7.59501135632552E-64,-4.62592926927149E-16));
#2117=DIRECTION('',(1.3103244120977E-47,-1.,2.83256473634769E-32));
#2118=DIRECTION('',(1.,-1.3103244120977E-47,-4.62592926927149E-16));
#2119=DIRECTION('',(1.3103244120977E-47,-1.,2.83256473634769E-32));
#2120=DIRECTION('',(1.,-1.3103244120977E-47,-4.62592926927149E-16));
#2121=DIRECTION('center_axis',(4.62592926927149E-16,2.83256473634769E-32,
1.));
#2122=DIRECTION('ref_axis',(1.,-7.59501135632552E-64,-4.62592926927149E-16));
#2123=DIRECTION('center_axis',(4.62592926927149E-16,2.83256473634769E-32,
1.));
#2124=DIRECTION('ref_axis',(1.,-7.59501135632552E-64,-4.62592926927149E-16));
#2125=DIRECTION('center_axis',(4.62592926927149E-16,2.83256473634769E-32,
1.));
#2126=DIRECTION('ref_axis',(1.,-7.59501135632552E-64,-4.62592926927149E-16));
#2127=DIRECTION('center_axis',(4.62592926927149E-16,2.83256473634769E-32,
1.));
#2128=DIRECTION('ref_axis',(1.,-7.59501135632552E-64,-4.62592926927149E-16));
#2129=DIRECTION('center_axis',(-4.62592926927149E-16,-2.83256473634769E-32,
-1.));
#2130=DIRECTION('ref_axis',(-1.,1.3103244120977E-47,4.62592926927149E-16));
#2131=DIRECTION('',(1.3103244120977E-47,-1.,2.83256473634769E-32));
#2132=DIRECTION('center_axis',(4.62592926927149E-16,2.83256473634769E-32,
1.));
#2133=DIRECTION('ref_axis',(1.,-7.59501135632552E-64,-4.62592926927149E-16));
#2134=DIRECTION('',(1.,-4.67973004320639E-49,-4.62592926927149E-16));
#2135=DIRECTION('center_axis',(4.62592926927149E-16,2.83256473634769E-32,
1.));
#2136=DIRECTION('ref_axis',(1.,-7.59501135632553E-64,-4.62592926927149E-16));
#2137=DIRECTION('',(1.3103244120977E-47,-1.,2.83256473634769E-32));
#2138=DIRECTION('center_axis',(4.62592926927149E-16,2.83256473634769E-32,
1.));
#2139=DIRECTION('ref_axis',(1.,-7.59501135632553E-64,-4.62592926927149E-16));
#2140=DIRECTION('',(1.,-4.67973004320639E-49,-4.62592926927149E-16));
#2141=DIRECTION('center_axis',(4.62592926927149E-16,2.83256473634769E-32,
1.));
#2142=DIRECTION('ref_axis',(1.,-7.59501135632552E-64,-4.62592926927149E-16));
#2143=DIRECTION('center_axis',(4.62592926927149E-16,2.83256473634769E-32,
1.));
#2144=DIRECTION('ref_axis',(1.,-7.59501135632552E-64,-4.62592926927149E-16));
#2145=DIRECTION('center_axis',(4.62592926927149E-16,2.83256473634769E-32,
1.));
#2146=DIRECTION('ref_axis',(1.,-7.59501135632552E-64,-4.62592926927149E-16));
#2147=DIRECTION('center_axis',(4.62592926927149E-16,2.83256473634769E-32,
1.));
#2148=DIRECTION('ref_axis',(1.,-7.59501135632552E-64,-4.62592926927149E-16));
#2149=DIRECTION('center_axis',(4.62592926927149E-16,2.83256473634769E-32,
1.));
#2150=DIRECTION('ref_axis',(1.,-7.59501135632552E-64,-4.62592926927149E-16));
#2151=DIRECTION('',(1.,-1.3103244120977E-47,-4.62592926927149E-16));
#2152=DIRECTION('',(1.3103244120977E-47,-1.,2.83256473634769E-32));
#2153=DIRECTION('',(1.,-1.3103244120977E-47,-4.62592926927149E-16));
#2154=DIRECTION('',(1.3103244120977E-47,-1.,2.83256473634769E-32));
#2155=DIRECTION('center_axis',(1.,0.,-4.62592926927149E-16));
#2156=DIRECTION('ref_axis',(4.62592926927149E-16,0.,1.));
#2157=DIRECTION('',(4.62592926927149E-16,2.83256473634769E-32,1.));
#2158=DIRECTION('',(4.62592926927149E-16,2.83256473634769E-32,1.));
#2159=DIRECTION('center_axis',(4.62592926927149E-16,2.83256473634769E-32,
1.));
#2160=DIRECTION('ref_axis',(-1.,7.59501135632552E-64,4.62592926927149E-16));
#2161=DIRECTION('',(4.62592926927149E-16,2.83256473634769E-32,1.));
#2162=DIRECTION('center_axis',(-1.26352711166564E-47,1.,-2.83256473634769E-32));
#2163=DIRECTION('ref_axis',(2.23962894278238E-95,2.83256473634769E-32,1.));
#2164=DIRECTION('',(4.62592926927149E-16,2.83256473634769E-32,1.));
#2165=DIRECTION('center_axis',(4.62592926927149E-16,2.83256473634769E-32,
1.));
#2166=DIRECTION('ref_axis',(-1.,7.59501135632553E-64,4.62592926927149E-16));
#2167=DIRECTION('',(4.62592926927149E-16,2.83256473634769E-32,1.));
#2168=DIRECTION('center_axis',(1.,0.,-4.62592926927149E-16));
#2169=DIRECTION('ref_axis',(4.62592926927149E-16,0.,1.));
#2170=DIRECTION('',(4.62592926927149E-16,2.83256473634769E-32,1.));
#2171=DIRECTION('center_axis',(4.62592926927149E-16,2.83256473634769E-32,
1.));
#2172=DIRECTION('ref_axis',(-1.,7.59501135632553E-64,4.62592926927149E-16));
#2173=DIRECTION('',(4.62592926927149E-16,2.83256473634769E-32,1.));
#2174=DIRECTION('center_axis',(-1.26352711166564E-47,1.,-2.83256473634769E-32));
#2175=DIRECTION('ref_axis',(2.23962894278238E-95,2.83256473634769E-32,1.));
#2176=DIRECTION('',(4.62592926927149E-16,2.83256473634769E-32,1.));
#2177=DIRECTION('center_axis',(4.62592926927149E-16,2.83256473634769E-32,
1.));
#2178=DIRECTION('ref_axis',(-1.,7.59501135632552E-64,4.62592926927149E-16));
#2179=DIRECTION('',(4.62592926927149E-16,2.83256473634769E-32,1.));
#2180=DIRECTION('center_axis',(4.62592926927149E-16,2.83256473634769E-32,
1.));
#2181=DIRECTION('ref_axis',(-1.,7.59501135632552E-64,4.62592926927149E-16));
#2182=DIRECTION('',(4.62592926927149E-16,2.83256473634769E-32,1.));
#2183=DIRECTION('center_axis',(4.62592926927149E-16,2.83256473634769E-32,
1.));
#2184=DIRECTION('ref_axis',(-1.,7.59501135632552E-64,4.62592926927149E-16));
#2185=DIRECTION('',(4.62592926927149E-16,2.83256473634769E-32,1.));
#2186=DIRECTION('center_axis',(4.62592926927149E-16,2.83256473634769E-32,
1.));
#2187=DIRECTION('ref_axis',(-1.,7.59501135632552E-64,4.62592926927149E-16));
#2188=DIRECTION('',(4.62592926927149E-16,2.83256473634769E-32,1.));
#2189=DIRECTION('center_axis',(4.62592926927149E-16,2.83256473634769E-32,
1.));
#2190=DIRECTION('ref_axis',(-1.,7.59501135632552E-64,4.62592926927149E-16));
#2191=DIRECTION('center_axis',(0.,1.,-2.83256473634769E-32));
#2192=DIRECTION('ref_axis',(0.,2.83256473634769E-32,1.));
#2193=DIRECTION('',(4.62592926927149E-16,2.83256473634769E-32,1.));
#2194=DIRECTION('',(4.62592926927149E-16,2.83256473634769E-32,1.));
#2195=DIRECTION('center_axis',(1.,0.,-4.62592926927149E-16));
#2196=DIRECTION('ref_axis',(-4.62592926927149E-16,0.,-1.));
#2197=DIRECTION('',(4.62592926927149E-16,2.83256473634769E-32,1.));
#2198=DIRECTION('center_axis',(0.,1.,-2.83256473634769E-32));
#2199=DIRECTION('ref_axis',(0.,2.83256473634769E-32,1.));
#2200=DIRECTION('',(4.62592926927149E-16,2.83256473634769E-32,1.));
#2201=DIRECTION('center_axis',(1.,0.,-4.62592926927149E-16));
#2202=DIRECTION('ref_axis',(-4.62592926927149E-16,0.,-1.));
#2203=DIRECTION('axis',(0.,0.,1.));
#2204=DIRECTION('refdir',(1.,0.,0.));
#2205=DIRECTION('center_axis',(-0.866025403784439,0.5,0.));
#2206=DIRECTION('ref_axis',(-0.5,-0.866025403784439,0.));
#2207=DIRECTION('',(0.,0.,-1.));
#2208=DIRECTION('',(0.,0.,-1.));
#2209=DIRECTION('center_axis',(-0.866025403784438,-0.5,0.));
#2210=DIRECTION('ref_axis',(0.5,-0.866025403784438,0.));
#2211=DIRECTION('',(0.,0.,-1.));
#2212=DIRECTION('center_axis',(0.,-1.,0.));
#2213=DIRECTION('ref_axis',(0.,0.,-1.));
#2214=DIRECTION('',(0.,0.,-1.));
#2215=DIRECTION('center_axis',(0.866025403784439,-0.5,0.));
#2216=DIRECTION('ref_axis',(0.5,0.866025403784439,0.));
#2217=DIRECTION('',(0.,0.,-1.));
#2218=DIRECTION('center_axis',(0.866025403784438,0.5,0.));
#2219=DIRECTION('ref_axis',(-0.5,0.866025403784438,0.));
#2220=DIRECTION('',(0.,0.,-1.));
#2221=DIRECTION('center_axis',(0.,1.,0.));
#2222=DIRECTION('ref_axis',(0.,0.,1.));
#2223=DIRECTION('center_axis',(0.,0.,-1.));
#2224=DIRECTION('ref_axis',(-1.,0.,0.));
#2225=DIRECTION('center_axis',(0.,0.,1.));
#2226=DIRECTION('ref_axis',(1.,0.,0.));
#2227=DIRECTION('center_axis',(0.,0.,-1.));
#2228=DIRECTION('ref_axis',(-1.,0.,0.));
#2229=DIRECTION('center_axis',(0.,0.,1.));
#2230=DIRECTION('ref_axis',(1.,0.,0.));
#2231=DIRECTION('center_axis',(0.,0.,-1.));
#2232=DIRECTION('ref_axis',(1.,1.22464679914735E-16,0.));
#2233=DIRECTION('center_axis',(0.,0.,1.));
#2234=DIRECTION('ref_axis',(1.,0.,0.));
#2235=DIRECTION('center_axis',(0.,0.,-1.));
#2236=DIRECTION('ref_axis',(-1.,0.,0.));
#2237=DIRECTION('center_axis',(0.,0.,1.));
#2238=DIRECTION('ref_axis',(1.,0.,0.));
#2239=DIRECTION('center_axis',(0.,0.,-1.));
#2240=DIRECTION('ref_axis',(-1.,0.,0.));
#2241=DIRECTION('center_axis',(0.,0.,1.));
#2242=DIRECTION('ref_axis',(1.,0.,0.));
#2243=DIRECTION('center_axis',(0.,0.,-1.));
#2244=DIRECTION('ref_axis',(-1.,0.,0.));
#2245=DIRECTION('center_axis',(0.,0.,1.));
#2246=DIRECTION('ref_axis',(1.,0.,0.));
#2247=DIRECTION('center_axis',(0.,0.,1.));
#2248=DIRECTION('ref_axis',(1.,0.,0.));
#2249=DIRECTION('center_axis',(0.,0.,1.));
#2250=DIRECTION('ref_axis',(1.,0.,0.));
#2251=DIRECTION('center_axis',(0.,0.,1.));
#2252=DIRECTION('ref_axis',(1.,0.,0.));
#2253=DIRECTION('center_axis',(0.,0.,1.));
#2254=DIRECTION('ref_axis',(1.,0.,0.));
#2255=DIRECTION('center_axis',(1.22464679914735E-16,-1.,0.));
#2256=DIRECTION('ref_axis',(-1.,-1.22464679914735E-16,0.));
#2257=DIRECTION('center_axis',(0.,0.,1.));
#2258=DIRECTION('ref_axis',(1.,0.,0.));
#2259=DIRECTION('center_axis',(0.,0.,-1.));
#2260=DIRECTION('ref_axis',(-1.,0.,0.));
#2261=DIRECTION('',(-0.939692620785908,1.15079156022785E-16,0.342020143325669));
#2262=DIRECTION('center_axis',(0.,0.,1.));
#2263=DIRECTION('ref_axis',(1.,0.,0.));
#2264=DIRECTION('center_axis',(0.,0.,1.));
#2265=DIRECTION('ref_axis',(1.,0.,0.));
#2266=DIRECTION('center_axis',(0.,0.,1.));
#2267=DIRECTION('ref_axis',(1.,0.,0.));
#2268=DIRECTION('center_axis',(0.,0.,1.));
#2269=DIRECTION('ref_axis',(1.,0.,0.));
#2270=DIRECTION('',(0.,0.,-1.));
#2271=DIRECTION('center_axis',(0.,0.,-1.));
#2272=DIRECTION('ref_axis',(-1.,0.,0.));
#2273=DIRECTION('center_axis',(0.,0.,-1.));
#2274=DIRECTION('ref_axis',(1.,0.,0.));
#2275=DIRECTION('center_axis',(0.,0.,-1.));
#2276=DIRECTION('ref_axis',(-1.,0.,0.));
#2277=DIRECTION('center_axis',(0.,0.,1.));
#2278=DIRECTION('ref_axis',(1.,0.,0.));
#2279=DIRECTION('center_axis',(-1.22464679914735E-16,1.,0.));
#2280=DIRECTION('ref_axis',(-1.,-1.22464679914735E-16,0.));
#2281=DIRECTION('center_axis',(0.,0.,1.));
#2282=DIRECTION('ref_axis',(1.,0.,0.));
#2283=DIRECTION('',(0.707106781186549,8.65956056235495E-17,-0.707106781186546));
#2284=DIRECTION('axis',(0.,0.,1.));
#2285=DIRECTION('refdir',(1.,0.,0.));
#2286=DIRECTION('center_axis',(0.,1.,0.));
#2287=DIRECTION('ref_axis',(0.,0.,1.));
#2288=DIRECTION('',(0.,0.,-1.));
#2289=DIRECTION('',(0.,0.,-1.));
#2290=DIRECTION('center_axis',(-0.866025403784438,0.5,0.));
#2291=DIRECTION('ref_axis',(-0.5,-0.866025403784438,0.));
#2292=DIRECTION('',(0.,0.,-1.));
#2293=DIRECTION('center_axis',(-0.866025403784438,-0.5,0.));
#2294=DIRECTION('ref_axis',(0.5,-0.866025403784438,0.));
#2295=DIRECTION('',(0.,0.,-1.));
#2296=DIRECTION('center_axis',(0.,-1.,0.));
#2297=DIRECTION('ref_axis',(0.,0.,-1.));
#2298=DIRECTION('',(0.,0.,-1.));
#2299=DIRECTION('center_axis',(0.866025403784439,-0.5,0.));
#2300=DIRECTION('ref_axis',(0.5,0.866025403784439,0.));
#2301=DIRECTION('',(0.,0.,-1.));
#2302=DIRECTION('center_axis',(0.866025403784438,0.5,0.));
#2303=DIRECTION('ref_axis',(-0.5,0.866025403784438,0.));
#2304=DIRECTION('center_axis',(0.,0.,1.));
#2305=DIRECTION('ref_axis',(1.,0.,0.));
#2306=DIRECTION('center_axis',(0.,0.,1.));
#2307=DIRECTION('ref_axis',(1.,0.,0.));
#2308=DIRECTION('center_axis',(0.,0.,1.));
#2309=DIRECTION('ref_axis',(1.,0.,0.));
#2310=DIRECTION('center_axis',(0.,0.,1.));
#2311=DIRECTION('ref_axis',(1.,0.,0.));
#2312=DIRECTION('center_axis',(0.,0.,1.));
#2313=DIRECTION('ref_axis',(1.,0.,0.));
#2314=DIRECTION('center_axis',(0.,0.,1.));
#2315=DIRECTION('ref_axis',(1.,0.,0.));
#2316=DIRECTION('center_axis',(0.,0.,1.));
#2317=DIRECTION('ref_axis',(1.,0.,0.));
#2318=DIRECTION('center_axis',(0.,0.,1.));
#2319=DIRECTION('ref_axis',(1.,0.,0.));
#2320=DIRECTION('center_axis',(0.,0.,-1.));
#2321=DIRECTION('ref_axis',(-1.,0.,0.));
#2322=DIRECTION('center_axis',(0.,0.,1.));
#2323=DIRECTION('ref_axis',(1.,0.,0.));
#2324=DIRECTION('',(0.,0.,-1.));
#2325=DIRECTION('center_axis',(0.,0.,1.));
#2326=DIRECTION('ref_axis',(1.,0.,0.));
#2327=DIRECTION('center_axis',(0.,0.,1.));
#2328=DIRECTION('ref_axis',(1.,0.,0.));
#2329=DIRECTION('center_axis',(0.,0.,1.));
#2330=DIRECTION('ref_axis',(1.,0.,0.));
#2331=DIRECTION('center_axis',(0.,0.,1.));
#2332=DIRECTION('ref_axis',(1.,0.,0.));
#2333=DIRECTION('center_axis',(0.,0.,1.));
#2334=DIRECTION('ref_axis',(1.,0.,0.));
#2335=DIRECTION('center_axis',(0.,0.,-1.));
#2336=DIRECTION('ref_axis',(1.,5.66553889764798E-16,0.));
#2337=DIRECTION('center_axis',(0.,0.,-1.));
#2338=DIRECTION('ref_axis',(-1.,0.,0.));
#2339=DIRECTION('center_axis',(0.,0.,-1.));
#2340=DIRECTION('ref_axis',(-1.,0.,0.));
#2341=DIRECTION('center_axis',(0.,0.,-1.));
#2342=DIRECTION('ref_axis',(-1.,0.,0.));
#2343=DIRECTION('center_axis',(0.,0.,-1.));
#2344=DIRECTION('ref_axis',(-1.,0.,0.));
#2345=DIRECTION('center_axis',(0.,0.,-1.));
#2346=DIRECTION('ref_axis',(-1.,0.,0.));
#2347=DIRECTION('center_axis',(0.,0.,-1.));
#2348=DIRECTION('ref_axis',(-1.,0.,0.));
#2349=DIRECTION('center_axis',(0.,0.,1.));
#2350=DIRECTION('ref_axis',(1.,0.,0.));
#2351=DIRECTION('',(-0.939692620785908,1.15079156022785E-16,0.342020143325669));
#2352=DIRECTION('center_axis',(0.,0.,1.));
#2353=DIRECTION('ref_axis',(1.,0.,0.));
#2354=DIRECTION('center_axis',(0.,0.,1.));
#2355=DIRECTION('ref_axis',(1.,0.,0.));
#2356=DIRECTION('center_axis',(1.22464679914735E-16,-1.,0.));
#2357=DIRECTION('ref_axis',(-1.,-1.22464679914735E-16,0.));
#2358=DIRECTION('center_axis',(0.,0.,-1.));
#2359=DIRECTION('ref_axis',(-1.,0.,0.));
#2360=DIRECTION('',(0.707106781186547,-8.65956056235493E-17,-0.707106781186548));
#2361=DIRECTION('center_axis',(0.,0.,1.));
#2362=DIRECTION('ref_axis',(1.,0.,0.));
#2363=DIRECTION('',(-0.707106781186547,-8.65956056235493E-17,0.707106781186548));
#2364=DIRECTION('axis',(0.,0.,1.));
#2365=DIRECTION('refdir',(1.,0.,0.));
#2366=DIRECTION('center_axis',(-1.,0.,0.));
#2367=DIRECTION('ref_axis',(0.,0.,-1.));
#2368=DIRECTION('center_axis',(-0.99372130819269,0.,-0.111883696952722));
#2369=DIRECTION('ref_axis',(-0.111883696952722,0.,0.99372130819269));
#2370=DIRECTION('',(-1.,0.,0.));
#2371=DIRECTION('center_axis',(0.994206946103325,0.,-0.107482781504297));
#2372=DIRECTION('ref_axis',(-0.107482781504297,0.,-0.994206946103325));
#2373=DIRECTION('center_axis',(-1.,0.,0.));
#2374=DIRECTION('ref_axis',(0.,0.,-1.));
#2375=DIRECTION('',(0.,-1.,0.));
#2376=DIRECTION('center_axis',(1.,0.,0.));
#2377=DIRECTION('ref_axis',(0.,0.,-1.));
#2378=DIRECTION('center_axis',(0.,-1.,0.));
#2379=DIRECTION('ref_axis',(0.,0.,1.));
#2380=DIRECTION('center_axis',(0.,-0.811541913546029,-0.5842942089034));
#2381=DIRECTION('ref_axis',(0.,-0.5842942089034,0.811541913546029));
#2382=DIRECTION('center_axis',(0.,0.978147600733806,0.207911690817759));
#2383=DIRECTION('ref_axis',(0.,-0.207911690817759,0.978147600733806));
#2384=DIRECTION('',(0.,-1.,0.));
#2385=DIRECTION('',(0.,-1.,0.));
#2386=DIRECTION('center_axis',(0.0838731411310077,0.675424884631005,-0.732643515918903));
#2387=DIRECTION('ref_axis',(0.993606931693314,-0.000929786476276916,0.112891101456694));
#2388=DIRECTION('center_axis',(0.99372130819269,0.,0.111883696952722));
#2389=DIRECTION('ref_axis',(-0.111883696952722,0.,0.99372130819269));
#2390=DIRECTION('',(0.109468391364691,0.206662199202023,-0.97226920485687));
#2391=DIRECTION('',(0.,-1.,0.));
#2392=DIRECTION('',(0.111883696952722,0.,-0.99372130819269));
#2393=DIRECTION('',(0.,-1.,0.));
#2394=DIRECTION('',(-0.111883696952722,0.,0.99372130819269));
#2395=DIRECTION('center_axis',(-1.,0.,0.));
#2396=DIRECTION('ref_axis',(0.,0.,-1.));
#2397=DIRECTION('',(0.,-1.,0.));
#2398=DIRECTION('center_axis',(1.,0.,0.));
#2399=DIRECTION('ref_axis',(0.,0.,-1.));
#2400=DIRECTION('center_axis',(1.,0.,0.));
#2401=DIRECTION('ref_axis',(0.,0.,1.));
#2402=DIRECTION('center_axis',(-1.,0.,0.));
#2403=DIRECTION('ref_axis',(0.,0.,1.));
#2404=DIRECTION('',(0.,-1.,0.));
#2405=DIRECTION('center_axis',(0.,-1.,0.));
#2406=DIRECTION('ref_axis',(0.,0.,1.));
#2407=DIRECTION('center_axis',(0.,0.978147600733806,0.207911690817759));
#2408=DIRECTION('ref_axis',(0.,-0.207911690817759,0.978147600733806));
#2409=DIRECTION('center_axis',(0.,-0.811541913546029,-0.5842942089034));
#2410=DIRECTION('ref_axis',(0.,-0.5842942089034,0.811541913546029));
#2411=DIRECTION('',(0.,-1.,0.));
#2412=DIRECTION('',(0.,-1.,0.));
#2413=DIRECTION('center_axis',(0.,-1.,0.));
#2414=DIRECTION('ref_axis',(0.,0.,1.));
#2415=DIRECTION('center_axis',(0.,0.978147600733806,0.207911690817759));
#2416=DIRECTION('ref_axis',(0.,-0.207911690817759,0.978147600733806));
#2417=DIRECTION('',(0.,-1.,0.));
#2418=DIRECTION('',(0.,-1.,0.));
#2419=DIRECTION('center_axis',(0.,-0.811541913546029,-0.5842942089034));
#2420=DIRECTION('ref_axis',(0.,-0.5842942089034,0.811541913546029));
#2421=DIRECTION('center_axis',(-0.994206946103325,0.,0.107482781504297));
#2422=DIRECTION('ref_axis',(-0.107482781504297,0.,-0.994206946103325));
#2423=DIRECTION('',(0.,-1.,0.));
#2424=DIRECTION('',(0.105160285869614,-0.206758879790012,0.972724051262125));
#2425=DIRECTION('',(-0.0873993054910777,0.582058324791578,-0.808436434075369));
#2426=DIRECTION('center_axis',(0.,-1.,0.));
#2427=DIRECTION('ref_axis',(7.6571373978539E-16,0.,-1.));
#2428=DIRECTION('center_axis',(0.,0.978147600733806,0.207911690817759));
#2429=DIRECTION('ref_axis',(0.,-0.207911690817759,0.978147600733806));
#2430=DIRECTION('center_axis',(0.,-0.811541913546029,-0.5842942089034));
#2431=DIRECTION('ref_axis',(0.,-0.5842942089034,0.811541913546029));
#2432=DIRECTION('',(0.,-1.,0.));
#2433=DIRECTION('center_axis',(-0.994206946103325,0.,-0.107482781504297));
#2434=DIRECTION('ref_axis',(0.107482781504297,0.,-0.994206946103325));
#2435=DIRECTION('',(-0.105160285869614,-0.206758879790012,0.972724051262125));
#2436=DIRECTION('',(0.0873993054910777,0.582058324791578,-0.808436434075369));
#2437=DIRECTION('center_axis',(0.994206946103325,0.,0.107482781504297));
#2438=DIRECTION('ref_axis',(-0.107482781504297,0.,0.994206946103325));
#2439=DIRECTION('center_axis',(0.,-1.,0.));
#2440=DIRECTION('ref_axis',(0.,0.,1.));
#2441=DIRECTION('',(-1.,0.,0.));
#2442=DIRECTION('',(0.111883696952722,0.,0.99372130819269));
#2443=DIRECTION('',(-1.,0.,0.));
#2444=DIRECTION('center_axis',(0.,0.,1.));
#2445=DIRECTION('ref_axis',(-1.,0.,0.));
#2446=DIRECTION('',(-1.,0.,0.));
#2447=DIRECTION('',(0.,1.,0.));
#2448=DIRECTION('center_axis',(0.,-0.978147600733806,-0.207911690817759));
#2449=DIRECTION('ref_axis',(0.,-0.207911690817759,0.978147600733806));
#2450=DIRECTION('',(-1.,0.,0.));
#2451=DIRECTION('center_axis',(0.,0.978147600733806,0.207911690817759));
#2452=DIRECTION('ref_axis',(0.,-0.207911690817759,0.978147600733806));
#2453=DIRECTION('',(0.109468391364691,-0.206662199202023,0.97226920485687));
#2454=DIRECTION('',(-1.,0.,0.));
#2455=DIRECTION('center_axis',(-1.,0.,0.));
#2456=DIRECTION('ref_axis',(0.,-0.404767724305038,0.914419536843412));
#2457=DIRECTION('',(-1.,0.,0.));
#2458=DIRECTION('center_axis',(-1.,0.,0.));
#2459=DIRECTION('ref_axis',(0.,-0.40476772430504,0.914419536843411));
#2460=DIRECTION('',(-1.,0.,0.));
#2461=DIRECTION('center_axis',(-1.,0.,0.));
#2462=DIRECTION('ref_axis',(0.,0.,1.));
#2463=DIRECTION('center_axis',(0.,0.811541913546029,0.5842942089034));
#2464=DIRECTION('ref_axis',(0.,0.5842942089034,-0.811541913546029));
#2465=DIRECTION('center_axis',(0.,-0.811541913546029,-0.5842942089034));
#2466=DIRECTION('ref_axis',(-0.137420443729346,0.578750897214899,-0.803842659118176));
#2467=DIRECTION('center_axis',(0.,-0.811541913546029,-0.5842942089034));
#2468=DIRECTION('ref_axis',(0.,-0.5842942089034,0.811541913546029));
#2469=DIRECTION('center_axis',(0.,-0.811541913546029,-0.5842942089034));
#2470=DIRECTION('ref_axis',(-0.137420443729346,-0.578750897214899,0.803842659118176));
#2471=DIRECTION('center_axis',(0.,0.,1.));
#2472=DIRECTION('ref_axis',(-1.,0.,0.));
#2473=DIRECTION('',(0.,-1.,0.));
#2474=DIRECTION('center_axis',(0.,0.,-1.));
#2475=DIRECTION('ref_axis',(-1.,0.,0.));
#2476=DIRECTION('center_axis',(0.,0.,-1.));
#2477=DIRECTION('ref_axis',(-1.,0.,0.));
#2478=DIRECTION('center_axis',(-1.,0.,0.));
#2479=DIRECTION('ref_axis',(0.,0.,-1.));
#2480=DIRECTION('',(-1.,0.,0.));
#2481=DIRECTION('center_axis',(0.99372130819269,0.,-0.111883696952722));
#2482=DIRECTION('ref_axis',(-0.111883696952722,0.,-0.99372130819269));
#2483=DIRECTION('center_axis',(1.,0.,0.));
#2484=DIRECTION('ref_axis',(0.,0.,1.));
#2485=DIRECTION('',(0.,-1.,0.));
#2486=DIRECTION('center_axis',(0.,-1.,0.));
#2487=DIRECTION('ref_axis',(0.,0.,1.));
#2488=DIRECTION('',(0.,-1.,0.));
#2489=DIRECTION('',(0.,-1.,0.));
#2490=DIRECTION('center_axis',(0.0838731194178255,-0.675424884481499,0.732643518542461));
#2491=DIRECTION('ref_axis',(-0.993606933527829,-0.000929771706171516,0.112891085431926));
#2492=DIRECTION('center_axis',(-0.99372130819269,0.,0.111883696952722));
#2493=DIRECTION('ref_axis',(-0.111883696952722,0.,-0.99372130819269));
#2494=DIRECTION('',(-0.111883696952722,0.,-0.99372130819269));
#2495=DIRECTION('center_axis',(-0.111883696952722,0.,-0.99372130819269));
#2496=DIRECTION('ref_axis',(0.99372130819269,0.,-0.111883696952722));
#2497=DIRECTION('center_axis',(1.,0.,0.));
#2498=DIRECTION('ref_axis',(0.,0.,1.));
#2499=DIRECTION('center_axis',(-0.111883696952722,0.,0.99372130819269));
#2500=DIRECTION('ref_axis',(-0.99372130819269,0.,-0.111883696952722));
#2501=DIRECTION('',(0.,0.,1.));
#2502=DIRECTION('',(1.,0.,0.));
#2503=DIRECTION('',(0.,0.,1.));
#2504=DIRECTION('',(1.,0.,0.));
#2505=DIRECTION('',(-7.52601449037733E-17,-1.42957338783288E-16,-1.));
#2506=DIRECTION('',(1.,1.0547118733939E-15,-7.52601449037734E-17));
#2507=DIRECTION('',(-7.40066201427226E-16,-1.42957338783288E-16,-1.));
#2508=DIRECTION('',(1.,3.88578058618804E-16,-7.40066201427226E-16));
#2509=DIRECTION('',(1.35907804936917E-62,1.42957338783288E-16,1.));
#2510=DIRECTION('',(1.,2.96317351790181E-31,-4.23607400472357E-47));
#2511=DIRECTION('',(3.26351384609149E-16,-1.42957338783288E-16,-1.));
#2512=DIRECTION('',(1.,6.24500451351652E-16,3.26351384609149E-16));
#2513=DIRECTION('',(8.94903179954374E-16,-1.42957338783288E-16,-1.));
#2514=DIRECTION('',(1.,-5.55111512312587E-17,8.94903179954374E-16));
#2515=DIRECTION('',(-6.65759343724301E-16,-1.42957338783288E-16,-1.));
#2516=DIRECTION('',(1.,4.99600361081319E-16,-6.65759343724301E-16));
#2517=DIRECTION('',(1.61833384335612E-62,1.42957338783288E-16,1.));
#2518=DIRECTION('',(1.,2.85694641159623E-31,-4.08421456048261E-47));
#2519=DIRECTION('',(-8.67069221566122E-63,1.42957338783288E-16,1.));
#2520=DIRECTION('',(1.,-5.33500946465298E-32,7.62678755450445E-48));
#2521=DIRECTION('',(6.06573312901231E-16,1.42957338783288E-16,1.));
#2522=DIRECTION('',(1.,4.44089209850066E-16,-6.06573312901231E-16));
#2523=DIRECTION('',(0.,0.,1.));
#2524=DIRECTION('',(1.,0.,0.));
#2525=CARTESIAN_POINT('',(0.,0.,0.));
#2526=CARTESIAN_POINT('',(0.,0.,0.));
#2527=CARTESIAN_POINT('Origin',(0.015875,0.,1.55530143491714E-18));
#2528=CARTESIAN_POINT('',(-0.01143,0.,-0.0254));
#2529=CARTESIAN_POINT('Origin',(-0.01143,0.,1.55530143491714E-18));
#2530=CARTESIAN_POINT('',(-0.015875,0.,-0.0254));
#2531=CARTESIAN_POINT('',(0.015875,-3.11060286983428E-18,-0.0254));
#2532=CARTESIAN_POINT('Origin',(-0.015875,0.,1.55530143491714E-18));
#2533=CARTESIAN_POINT('Origin',(0.015875,0.,1.55530143491714E-18));
#2534=CARTESIAN_POINT('',(0.015875,0.,-0.0254));
#2535=CARTESIAN_POINT('Origin',(0.015875,0.,1.55530143491714E-18));
#2536=CARTESIAN_POINT('',(0.01143,0.,-0.0254));
#2537=CARTESIAN_POINT('',(0.015875,-3.11060286983428E-18,-0.0254));
#2538=CARTESIAN_POINT('Origin',(0.01143,0.,1.55530143491714E-18));
#2539=CARTESIAN_POINT('Origin',(0.015875,0.,2.33295215237571E-18));
#2540=CARTESIAN_POINT('',(-0.015875,0.,-0.0381));
#2541=CARTESIAN_POINT('Origin',(-0.015875,0.,2.33295215237571E-18));
#2542=CARTESIAN_POINT('',(0.015875,0.,-0.0381));
#2543=CARTESIAN_POINT('',(0.015875,-4.66590430475142E-18,-0.0381));
#2544=CARTESIAN_POINT('Origin',(0.015875,0.,2.33295215237571E-18));
#2545=CARTESIAN_POINT('Origin',(0.015875,0.,0.));
#2546=CARTESIAN_POINT('Origin',(-0.015875,0.,0.));
#2547=CARTESIAN_POINT('Origin',(0.01143,0.,4.66590430475142E-19));
#2548=CARTESIAN_POINT('',(0.01143,0.,-0.00762));
#2549=CARTESIAN_POINT('Origin',(0.01143,0.,4.66590430475142E-19));
#2550=CARTESIAN_POINT('',(-0.01143,0.,-0.00762));
#2551=CARTESIAN_POINT('',(0.01143,-9.33180860950283E-19,-0.00762));
#2552=CARTESIAN_POINT('Origin',(-0.01143,0.,4.66590430475142E-19));
#2553=CARTESIAN_POINT('Origin',(0.01143,0.,0.));
#2554=CARTESIAN_POINT('Origin',(-0.01143,0.,0.));
#2555=CARTESIAN_POINT('',(0.,0.,0.));
#2556=CARTESIAN_POINT('Origin',(0.03556,4.66590430475142E-19,0.));
#2557=CARTESIAN_POINT('',(-0.03556,4.66590430475142E-19,-0.00762));
#2558=CARTESIAN_POINT('Origin',(-0.03556,4.66590430475142E-19,0.));
#2559=CARTESIAN_POINT('',(0.03556,4.66590430475142E-19,-0.00762));
#2560=CARTESIAN_POINT('',(0.03556,-4.66590430475141E-19,-0.00762));
#2561=CARTESIAN_POINT('Origin',(0.03556,4.66590430475142E-19,0.));
#2562=CARTESIAN_POINT('Origin',(0.03556,0.,0.));
#2563=CARTESIAN_POINT('Origin',(-0.03556,0.,0.));
#2564=CARTESIAN_POINT('',(0.,0.,0.));
#2565=CARTESIAN_POINT('Origin',(0.45,-0.85,-0.031));
#2566=CARTESIAN_POINT('',(0.405,-0.815,-0.031));
#2567=CARTESIAN_POINT('',(0.405,-0.885,-0.031));
#2568=CARTESIAN_POINT('',(0.405,-0.85,-0.031));
#2569=CARTESIAN_POINT('',(0.415,-0.805,-0.031));
#2570=CARTESIAN_POINT('Origin',(0.415,-0.815,-0.031));
#2571=CARTESIAN_POINT('',(0.485,-0.805,-0.031));
#2572=CARTESIAN_POINT('',(0.45,-0.805,-0.031));
#2573=CARTESIAN_POINT('',(0.495,-0.815,-0.031));
#2574=CARTESIAN_POINT('Origin',(0.485,-0.815,-0.031));
#2575=CARTESIAN_POINT('',(0.495,-0.885,-0.031));
#2576=CARTESIAN_POINT('',(0.495,-0.85,-0.031));
#2577=CARTESIAN_POINT('',(0.485,-0.895,-0.031));
#2578=CARTESIAN_POINT('Origin',(0.485,-0.885,-0.031));
#2579=CARTESIAN_POINT('',(0.415,-0.895,-0.031));
#2580=CARTESIAN_POINT('',(0.45,-0.895,-0.031));
#2581=CARTESIAN_POINT('Origin',(0.415,-0.885,-0.031));
#2582=CARTESIAN_POINT('',(0.4475,-0.8425,-0.031));
#2583=CARTESIAN_POINT('',(0.4475,-0.8575,-0.031));
#2584=CARTESIAN_POINT('',(0.4475,-0.85,-0.031));
#2585=CARTESIAN_POINT('',(0.4525,-0.8575,-0.031));
#2586=CARTESIAN_POINT('',(0.45,-0.8575,-0.031));
#2587=CARTESIAN_POINT('',(0.4525,-0.8425,-0.031));
#2588=CARTESIAN_POINT('',(0.4525,-0.85,-0.031));
#2589=CARTESIAN_POINT('',(0.45,-0.8425,-0.031));
#2590=CARTESIAN_POINT('',(0.4195,-0.885,-0.031));
#2591=CARTESIAN_POINT('Origin',(0.415,-0.885,-0.031));
#2592=CARTESIAN_POINT('',(0.421185503721238,-0.815,-0.031));
#2593=CARTESIAN_POINT('Origin',(0.416685503721238,-0.815,-0.031));
#2594=CARTESIAN_POINT('',(0.4895,-0.815,-0.031));
#2595=CARTESIAN_POINT('Origin',(0.485,-0.815,-0.031));
#2596=CARTESIAN_POINT('',(0.4895,-0.885,-0.031));
#2597=CARTESIAN_POINT('Origin',(0.485,-0.885,-0.031));
#2598=CARTESIAN_POINT('Origin',(0.45,-0.85,-0.025));
#2599=CARTESIAN_POINT('',(0.405,-0.815,-0.025));
#2600=CARTESIAN_POINT('',(0.405,-0.885,-0.025));
#2601=CARTESIAN_POINT('',(0.405,-0.85,-0.025));
#2602=CARTESIAN_POINT('',(0.415,-0.895,-0.025));
#2603=CARTESIAN_POINT('Origin',(0.415,-0.885,-0.025));
#2604=CARTESIAN_POINT('',(0.485,-0.895,-0.025));
#2605=CARTESIAN_POINT('',(0.45,-0.895,-0.025));
#2606=CARTESIAN_POINT('',(0.495,-0.885,-0.025));
#2607=CARTESIAN_POINT('Origin',(0.485,-0.885,-0.025));
#2608=CARTESIAN_POINT('',(0.495,-0.815,-0.025));
#2609=CARTESIAN_POINT('',(0.495,-0.85,-0.025));
#2610=CARTESIAN_POINT('',(0.485,-0.805,-0.025));
#2611=CARTESIAN_POINT('Origin',(0.485,-0.815,-0.025));
#2612=CARTESIAN_POINT('',(0.415,-0.805,-0.025));
#2613=CARTESIAN_POINT('',(0.45,-0.805,-0.025));
#2614=CARTESIAN_POINT('Origin',(0.415,-0.815,-0.025));
#2615=CARTESIAN_POINT('',(0.4895,-0.885,-0.025));
#2616=CARTESIAN_POINT('Origin',(0.485,-0.885,-0.025));
#2617=CARTESIAN_POINT('',(0.4895,-0.815,-0.025));
#2618=CARTESIAN_POINT('Origin',(0.485,-0.815,-0.025));
#2619=CARTESIAN_POINT('',(0.421185503721238,-0.815,-0.025));
#2620=CARTESIAN_POINT('Origin',(0.416685503721238,-0.815,-0.025));
#2621=CARTESIAN_POINT('',(0.4195,-0.885,-0.025));
#2622=CARTESIAN_POINT('Origin',(0.415,-0.885,-0.025));
#2623=CARTESIAN_POINT('',(0.4475,-0.8575,-0.025));
#2624=CARTESIAN_POINT('',(0.4525,-0.8575,-0.025));
#2625=CARTESIAN_POINT('',(0.45,-0.8575,-0.025));
#2626=CARTESIAN_POINT('',(0.4475,-0.8425,-0.025));
#2627=CARTESIAN_POINT('',(0.4475,-0.85,-0.025));
#2628=CARTESIAN_POINT('',(0.4525,-0.8425,-0.025));
#2629=CARTESIAN_POINT('',(0.45,-0.8425,-0.025));
#2630=CARTESIAN_POINT('',(0.4525,-0.85,-0.025));
#2631=CARTESIAN_POINT('Origin',(0.405,-0.85,-0.031));
#2632=CARTESIAN_POINT('',(0.405,-0.815,-0.031));
#2633=CARTESIAN_POINT('',(0.405,-0.885,-0.031));
#2634=CARTESIAN_POINT('Origin',(0.415,-0.885,-0.031));
#2635=CARTESIAN_POINT('',(0.415,-0.895,-0.031));
#2636=CARTESIAN_POINT('Origin',(0.45,-0.895,-0.031));
#2637=CARTESIAN_POINT('',(0.485,-0.895,-0.031));
#2638=CARTESIAN_POINT('Origin',(0.485,-0.885,-0.031));
#2639=CARTESIAN_POINT('',(0.495,-0.885,-0.031));
#2640=CARTESIAN_POINT('Origin',(0.495,-0.85,-0.031));
#2641=CARTESIAN_POINT('',(0.495,-0.815,-0.031));
#2642=CARTESIAN_POINT('Origin',(0.485,-0.815,-0.031));
#2643=CARTESIAN_POINT('',(0.485,-0.805,-0.031));
#2644=CARTESIAN_POINT('Origin',(0.45,-0.805,-0.031));
#2645=CARTESIAN_POINT('',(0.415,-0.805,-0.031));
#2646=CARTESIAN_POINT('Origin',(0.485,-0.885,-0.031));
#2647=CARTESIAN_POINT('',(0.4895,-0.885,-0.031));
#2648=CARTESIAN_POINT('Origin',(0.485,-0.815,-0.031));
#2649=CARTESIAN_POINT('',(0.4895,-0.815,-0.031));
#2650=CARTESIAN_POINT('Origin',(0.416685503721238,-0.815,-0.031));
#2651=CARTESIAN_POINT('',(0.421185503721238,-0.815,-0.031));
#2652=CARTESIAN_POINT('Origin',(0.415,-0.885,-0.031));
#2653=CARTESIAN_POINT('',(0.4195,-0.885,-0.031));
#2654=CARTESIAN_POINT('Origin',(0.415,-0.815,-0.031));
#2655=CARTESIAN_POINT('Origin',(0.45,-0.8575,-0.058));
#2656=CARTESIAN_POINT('',(0.4475,-0.8575,-0.058));
#2657=CARTESIAN_POINT('',(0.4525,-0.8575,-0.058));
#2658=CARTESIAN_POINT('Origin',(0.4525,-0.85,-0.058));
#2659=CARTESIAN_POINT('',(0.4525,-0.8425,-0.058));
#2660=CARTESIAN_POINT('Origin',(0.45,-0.8425,-0.058));
#2661=CARTESIAN_POINT('',(0.4475,-0.8425,-0.058));
#2662=CARTESIAN_POINT('Origin',(0.4475,-0.85,-0.058));
#2663=CARTESIAN_POINT('',(0.,0.,0.));
#2664=CARTESIAN_POINT('Origin',(-0.00346410161513775,0.002,0.0068));
#2665=CARTESIAN_POINT('',(-0.00230940107675851,0.004,0.00644273441009184));
#2666=CARTESIAN_POINT('',(-0.00230939436406612,0.00399999494215664,0.0022625182008993));
#2667=CARTESIAN_POINT('',(-0.00230940107675851,0.004,0.0068));
#2668=CARTESIAN_POINT('',(-0.00461879440075555,3.31248999445318E-9,0.00226251801022537));
#2669=CARTESIAN_POINT('Ctrl Pts',(-0.00230940691705295,0.00399998988431329,
0.00226254053913407));
#2670=CARTESIAN_POINT('Ctrl Pts',(-0.00250052112625622,0.00366897036392486,
0.00232700363594611));
#2671=CARTESIAN_POINT('Ctrl Pts',(-0.00269262130445346,0.003336243093075,
0.0023789007474104));
#2672=CARTESIAN_POINT('Ctrl Pts',(-0.00288523530706997,0.00300262585845459,
0.00241461216933165));
#2673=CARTESIAN_POINT('Ctrl Pts',(-0.00307488976811388,0.00267413470014111,
0.00244977488017086));
#2674=CARTESIAN_POINT('Ctrl Pts',(-0.00326504319652788,0.00234477935046048,
0.00246919460122286));
#2675=CARTESIAN_POINT('Ctrl Pts',(-0.00345519948963801,0.00201541895392153,
0.00246969208645218));
#2676=CARTESIAN_POINT('Ctrl Pts',(-0.00345816686225689,0.00201027931322677,
0.00246969984966645));
#2677=CARTESIAN_POINT('Ctrl Pts',(-0.00346113423804048,0.00200513966704103,
0.00246970300391286));
#2678=CARTESIAN_POINT('Ctrl Pts',(-0.00346410161390816,0.00200000002070232,
0.00246970156489889));
#2679=CARTESIAN_POINT('Ctrl Pts',(-0.00365722549107684,0.00166549961614694,
0.00246960791044814));
#2680=CARTESIAN_POINT('Ctrl Pts',(-0.00385033581825397,0.00133102273658184,
0.0024498267811737));
#2681=CARTESIAN_POINT('Ctrl Pts',(-0.00404294431061013,0.000997415041851726,
0.00241413900952665));
#2682=CARTESIAN_POINT('Ctrl Pts',(-0.00423555280296629,0.000663807347121617,
0.00237845123787961));
#2683=CARTESIAN_POINT('Ctrl Pts',(-0.00442766851201852,0.000331053178111033,
0.00232683813848012));
#2684=CARTESIAN_POINT('Ctrl Pts',(-0.00461879248828856,1.67406667220262E-8,
0.00226249548131684));
#2685=CARTESIAN_POINT('',(-0.00461880215351701,8.67361737988403E-19,0.00644273441009184));
#2686=CARTESIAN_POINT('',(-0.00461880215351701,4.33680868994202E-19,0.0068));
#2687=CARTESIAN_POINT('',(-0.00346410161513775,0.002,0.0068));
#2688=CARTESIAN_POINT('Ctrl Pts',(-0.00461880215350316,2.39844418489033E-14,
0.00644273441009984));
#2689=CARTESIAN_POINT('Ctrl Pts',(-0.00399999999999443,0.00107179676973413,
0.0068));
#2690=CARTESIAN_POINT('Ctrl Pts',(-0.00346410161513775,0.00199999999999999,
0.0068));
#2691=CARTESIAN_POINT('Ctrl Pts',(-0.00346410161513775,0.00199999999999999,
0.0068));
#2692=CARTESIAN_POINT('Ctrl Pts',(-0.00292820323026226,0.00292820323029845,
0.0068));
#2693=CARTESIAN_POINT('Ctrl Pts',(-0.00230940107672554,0.00400000000005709,
0.00644273441007281));
#2694=CARTESIAN_POINT('Origin',(-0.00346410161513775,-0.002,0.0068));
#2695=CARTESIAN_POINT('',(-0.00230940010168572,-0.00399999162966664,0.00226251820212234));
#2696=CARTESIAN_POINT('Ctrl Pts',(-0.00461879631322255,-1.01156867331198E-8,
0.0022625405391339));
#2697=CARTESIAN_POINT('Ctrl Pts',(-0.00442768210401926,-0.000331029636075182,
0.00232700363594575));
#2698=CARTESIAN_POINT('Ctrl Pts',(-0.00423558192403004,-0.000663756905890421,
0.00237890074741006));
#2699=CARTESIAN_POINT('Ctrl Pts',(-0.00404296792501672,-0.000997374142591104,
0.00241461216933148));
#2700=CARTESIAN_POINT('Ctrl Pts',(-0.00385331346752063,-0.0013258653029529,
0.00244977488017086));
#2701=CARTESIAN_POINT('Ctrl Pts',(-0.00366316008203189,-0.00165522067741645,
0.00246919460122286));
#2702=CARTESIAN_POINT('Ctrl Pts',(-0.00347300375818371,-0.00198458105620877,
0.00246969208645221));
#2703=CARTESIAN_POINT('Ctrl Pts',(-0.00347003638508517,-0.0019897206966266,
0.00246969984966648));
#2704=CARTESIAN_POINT('Ctrl Pts',(-0.00346706900881365,-0.00199486034253063,
0.00246970300391289));
#2705=CARTESIAN_POINT('Ctrl Pts',(-0.0034641016324517,-0.00199999998858397,
0.00246970156489892));
#2706=CARTESIAN_POINT('Ctrl Pts',(-0.0032709777231149,-0.00233450037456709,
0.0024696079104482));
#2707=CARTESIAN_POINT('Ctrl Pts',(-0.00307786741202155,-0.00266897726341815,
0.00244982678117377));
#2708=CARTESIAN_POINT('Ctrl Pts',(-0.00288525891966538,-0.00300258495814827,
0.00241413900952672));
#2709=CARTESIAN_POINT('Ctrl Pts',(-0.00269265042730922,-0.00333619265287839,
0.00237845123787968));
#2710=CARTESIAN_POINT('Ctrl Pts',(-0.00250053471825699,-0.00366894682188897,
0.00232683813848018));
#2711=CARTESIAN_POINT('Ctrl Pts',(-0.00230941074198694,-0.00399998325933328,
0.00226249548131687));
#2712=CARTESIAN_POINT('',(-0.00230940107675851,-0.004,0.00644273441009184));
#2713=CARTESIAN_POINT('',(-0.0023094010767585,-0.004,0.0068));
#2714=CARTESIAN_POINT('',(-0.00346410161513775,-0.002,0.0068));
#2715=CARTESIAN_POINT('Ctrl Pts',(-0.00230940107677235,-0.003999999999976,
0.00644273441009984));
#2716=CARTESIAN_POINT('Ctrl Pts',(-0.00292820323028107,-0.00292820323026586,
0.0068));
#2717=CARTESIAN_POINT('Ctrl Pts',(-0.00346410161513775,-0.002,0.0068));
#2718=CARTESIAN_POINT('Ctrl Pts',(-0.00346410161513775,-0.002,0.0068));
#2719=CARTESIAN_POINT('Ctrl Pts',(-0.00400000000001325,-0.00107179676970153,
0.0068));
#2720=CARTESIAN_POINT('Ctrl Pts',(-0.00461880215354998,5.71219321355913E-14,
0.0064427344100728));
#2721=CARTESIAN_POINT('Origin',(1.86807858924195E-18,-0.004,0.0068));
#2722=CARTESIAN_POINT('',(0.00230939429934915,-0.00399999494215665,0.00226251781990864));
#2723=CARTESIAN_POINT('Ctrl Pts',(-0.0023093894613845,-0.004,0.00226254092292782));
#2724=CARTESIAN_POINT('Ctrl Pts',(-0.00192716228032193,-0.004,0.00232700487022803));
#2725=CARTESIAN_POINT('Ctrl Pts',(-0.00154296885754916,-0.00399999999884996,
0.00237890343398045));
#2726=CARTESIAN_POINT('Ctrl Pts',(-0.00115774723711367,-0.00400000000116236,
0.002414613419996));
#2727=CARTESIAN_POINT('Ctrl Pts',(-0.000778474176435409,-0.00400000000343905,
0.00244977197542076));
#2728=CARTESIAN_POINT('Ctrl Pts',(-0.000398203312159713,-0.00400000002845795,
0.00246919150443257));
#2729=CARTESIAN_POINT('Ctrl Pts',(-1.79205700010576E-5,-0.00400000001033966,
0.00246969098913674));
#2730=CARTESIAN_POINT('Ctrl Pts',(-1.19561742901489E-5,-0.00400000001005549,
0.00246969882310893));
#2731=CARTESIAN_POINT('Ctrl Pts',(-5.99177071537931E-6,-0.00400000000976655,
0.00246970200182142));
#2732=CARTESIAN_POINT('Ctrl Pts',(-2.7365606690663E-8,-0.00400000000947396,
0.002469700541216));
#2733=CARTESIAN_POINT('Ctrl Pts',(0.000386220380851912,-0.00399999999052638,
0.00246960595415449));
#2734=CARTESIAN_POINT('Ctrl Pts',(0.000772447112493431,-0.004,0.00244982367082224));
#2735=CARTESIAN_POINT('Ctrl Pts',(0.00115767059475419,-0.004,0.00241413610794756));
#2736=CARTESIAN_POINT('Ctrl Pts',(0.00154289407701495,-0.004,0.00237844854507288));
#2737=CARTESIAN_POINT('Ctrl Pts',(0.00192713248193255,-0.004,0.00232683691852284));
#2738=CARTESIAN_POINT('Ctrl Pts',(0.00230938168164535,-0.004,0.00226249510068321));
#2739=CARTESIAN_POINT('',(0.0023094010767585,-0.004,0.00644273441009184));
#2740=CARTESIAN_POINT('',(0.00230940107675851,-0.004,0.0068));
#2741=CARTESIAN_POINT('',(0.,-0.004,0.0068));
#2742=CARTESIAN_POINT('Ctrl Pts',(-2.36670764249305E-18,-0.004,0.0068));
#2743=CARTESIAN_POINT('Ctrl Pts',(0.00107179676971335,-0.004,0.0068));
#2744=CARTESIAN_POINT('Ctrl Pts',(0.0023094010767308,-0.004,0.00644273441009984));
#2745=CARTESIAN_POINT('Ctrl Pts',(-0.00230940107682444,-0.004,0.0064427344100728));
#2746=CARTESIAN_POINT('Ctrl Pts',(-0.001071796769751,-0.004,0.0068));
#2747=CARTESIAN_POINT('Ctrl Pts',(-2.36670764249305E-18,-0.004,0.0068));
#2748=CARTESIAN_POINT('Origin',(0.00346410161513775,-0.002,0.0068));
#2749=CARTESIAN_POINT('',(0.00461879440075556,-3.31249001825354E-9,0.00226251801022538));
#2750=CARTESIAN_POINT('Ctrl Pts',(0.00230940691705295,-0.00399998988431329,
0.00226254053913407));
#2751=CARTESIAN_POINT('Ctrl Pts',(0.00250052112625622,-0.00366897036392487,
0.00232700363594613));
#2752=CARTESIAN_POINT('Ctrl Pts',(0.00269262130445346,-0.00333624309307501,
0.00237890074741045));
#2753=CARTESIAN_POINT('Ctrl Pts',(0.00288523530706997,-0.0030026258584546,
0.00241461216933168));
#2754=CARTESIAN_POINT('Ctrl Pts',(0.00307488976811388,-0.00267413470014111,
0.00244977488017086));
#2755=CARTESIAN_POINT('Ctrl Pts',(0.00326504319652788,-0.00234477935046048,
0.00246919460122286));
#2756=CARTESIAN_POINT('Ctrl Pts',(0.00345519948963801,-0.00201541895392154,
0.00246969208645215));
#2757=CARTESIAN_POINT('Ctrl Pts',(0.00345816686225689,-0.00201027931322678,
0.00246969984966642));
#2758=CARTESIAN_POINT('Ctrl Pts',(0.00346113423804048,-0.00200513966704103,
0.00246970300391282));
#2759=CARTESIAN_POINT('Ctrl Pts',(0.00346410161390816,-0.00200000002070232,
0.00246970156489885));
#2760=CARTESIAN_POINT('Ctrl Pts',(0.00365722549107684,-0.00166549961614694,
0.00246960791044806));
#2761=CARTESIAN_POINT('Ctrl Pts',(0.00385033581825397,-0.00133102273658185,
0.00244982678117351));
#2762=CARTESIAN_POINT('Ctrl Pts',(0.00404294431061012,-0.000997415041851751,
0.0024141390095264));
#2763=CARTESIAN_POINT('Ctrl Pts',(0.00423555280296627,-0.000663807347121655,
0.0023784512378793));
#2764=CARTESIAN_POINT('Ctrl Pts',(0.00442766851201849,-0.000331053178111084,
0.00232683813847981));
#2765=CARTESIAN_POINT('Ctrl Pts',(0.00461879248828856,-1.67406667481163E-8,
0.0022624954813167));
#2766=CARTESIAN_POINT('',(0.00461880215351701,0.,0.00644273441009184));
#2767=CARTESIAN_POINT('',(0.00461880215351701,0.,0.0068));
#2768=CARTESIAN_POINT('',(0.00346410161513775,-0.002,0.0068));
#2769=CARTESIAN_POINT('Ctrl Pts',(0.00461880215350315,-2.3987204103231E-14,
0.00644273441009984));
#2770=CARTESIAN_POINT('Ctrl Pts',(0.00399999999999443,-0.00107179676973414,
0.0068));
#2771=CARTESIAN_POINT('Ctrl Pts',(0.00346410161513775,-0.00200000000000001,
0.0068));
#2772=CARTESIAN_POINT('Ctrl Pts',(0.00346410161513775,-0.00200000000000001,
0.0068));
#2773=CARTESIAN_POINT('Ctrl Pts',(0.00292820323026226,-0.00292820323029846,
0.0068));
#2774=CARTESIAN_POINT('Ctrl Pts',(0.00230940107672555,-0.00400000000005708,
0.00644273441007281));
#2775=CARTESIAN_POINT('Origin',(0.00346410161513775,0.002,0.0068));
#2776=CARTESIAN_POINT('',(0.00230940003642643,0.00399999162966663,0.00226251781806703));
#2777=CARTESIAN_POINT('Ctrl Pts',(0.00461879631322256,1.01156867116092E-8,
0.00226254053913407));
#2778=CARTESIAN_POINT('Ctrl Pts',(0.00442768210401929,0.000331029636075126,
0.00232700363594612));
#2779=CARTESIAN_POINT('Ctrl Pts',(0.00423558192403006,0.000663756905890381,
0.00237890074741046));
#2780=CARTESIAN_POINT('Ctrl Pts',(0.00404296792501673,0.000997374142591087,
0.00241461216933168));
#2781=CARTESIAN_POINT('Ctrl Pts',(0.00385331346752063,0.0013258653029529,
0.00244977488017086));
#2782=CARTESIAN_POINT('Ctrl Pts',(0.0036631600820319,0.00165522067741644,
0.00246919460122286));
#2783=CARTESIAN_POINT('Ctrl Pts',(0.00347300375818372,0.00198458105620877,
0.00246969208645216));
#2784=CARTESIAN_POINT('Ctrl Pts',(0.00347003638508517,0.00198972069662659,
0.00246969984966643));
#2785=CARTESIAN_POINT('Ctrl Pts',(0.00346706900881365,0.00199486034253063,
0.00246970300391284));
#2786=CARTESIAN_POINT('Ctrl Pts',(0.0034641016324517,0.00199999998858397,
0.00246970156489887));
#2787=CARTESIAN_POINT('Ctrl Pts',(0.00327097772311491,0.00233450037456708,
0.00246960791044809));
#2788=CARTESIAN_POINT('Ctrl Pts',(0.00307786741202155,0.00266897726341816,
0.00244982678117361));
#2789=CARTESIAN_POINT('Ctrl Pts',(0.00288525891966539,0.00300258495814827,
0.00241413900952655));
#2790=CARTESIAN_POINT('Ctrl Pts',(0.00269265042730923,0.00333619265287837,
0.00237845123787949));
#2791=CARTESIAN_POINT('Ctrl Pts',(0.002500534718257,0.00366894682188895,
0.00232683813848));
#2792=CARTESIAN_POINT('Ctrl Pts',(0.00230941074198695,0.00399998325933327,
0.00226249548131679));
#2793=CARTESIAN_POINT('',(0.00230940107675851,0.004,0.00644273441009184));
#2794=CARTESIAN_POINT('',(0.00230940107675851,0.004,0.0068));
#2795=CARTESIAN_POINT('',(0.00346410161513775,0.002,0.0068));
#2796=CARTESIAN_POINT('Ctrl Pts',(0.00230940107677235,0.003999999999976,
0.00644273441009984));
#2797=CARTESIAN_POINT('Ctrl Pts',(0.00292820323028107,0.00292820323026587,
0.0068));
#2798=CARTESIAN_POINT('Ctrl Pts',(0.00346410161513774,0.00200000000000001,
0.0068));
#2799=CARTESIAN_POINT('Ctrl Pts',(0.00346410161513774,0.00200000000000001,
0.0068));
#2800=CARTESIAN_POINT('Ctrl Pts',(0.00400000000001324,0.00107179676970155,
0.00680000000000001));
#2801=CARTESIAN_POINT('Ctrl Pts',(0.00461880215354997,-5.70991966576601E-14,
0.00644273441007281));
#2802=CARTESIAN_POINT('Origin',(0.,0.004,0.0068));
#2803=CARTESIAN_POINT('Ctrl Pts',(0.00230938933086591,0.004,0.00226254015481727));
#2804=CARTESIAN_POINT('Ctrl Pts',(0.00192715966343552,0.004,0.00232700240167072));
#2805=CARTESIAN_POINT('Ctrl Pts',(0.00154295236666105,0.00399999999907498,
0.00237889805720109));
#2806=CARTESIAN_POINT('Ctrl Pts',(0.00115771798562292,0.00400000000093493,
0.00241461091731328));
#2807=CARTESIAN_POINT('Ctrl Pts',(0.00077837318028794,0.00400000000276645,
0.00244977778879215));
#2808=CARTESIAN_POINT('Ctrl Pts',(0.000398030391648709,0.00400000002730032,
0.00246919770092989));
#2809=CARTESIAN_POINT('Ctrl Pts',(1.76878773571683E-5,0.00400000000992256,
0.00246969318518198));
#2810=CARTESIAN_POINT('Ctrl Pts',(1.1782811571249E-5,0.00400000000965276,
0.0024697008778984));
#2811=CARTESIAN_POINT('Ctrl Pts',(5.87774094490613E-6,0.00400000000937819,
0.00246970400775273));
#2812=CARTESIAN_POINT('Ctrl Pts',(-2.73285226471042E-8,0.00400000000909995,
0.00246970259022018));
#2813=CARTESIAN_POINT('Ctrl Pts',(-0.000386275149414076,0.00399999999090037,
0.00246960987008162));
#2814=CARTESIAN_POINT('Ctrl Pts',(-0.000772489689067513,0.004,0.00244982989983513));
#2815=CARTESIAN_POINT('Ctrl Pts',(-0.00115770017497109,0.004,0.00241414191963193));
#2816=CARTESIAN_POINT('Ctrl Pts',(-0.00154291066087466,0.004,0.00237845393942873));
#2817=CARTESIAN_POINT('Ctrl Pts',(-0.00192713509457193,0.004,0.00232683936300356));
#2818=CARTESIAN_POINT('Ctrl Pts',(-0.00230938181107929,0.004,0.00226249586266454));
#2819=CARTESIAN_POINT('',(0.,0.004,0.0068));
#2820=CARTESIAN_POINT('Ctrl Pts',(-0.00230940107673081,0.004,0.00644273441009983));
#2821=CARTESIAN_POINT('Ctrl Pts',(-0.00107179676971336,0.004,0.0068));
#2822=CARTESIAN_POINT('Ctrl Pts',(1.18335392355646E-17,0.004,0.0068));
#2823=CARTESIAN_POINT('Ctrl Pts',(1.18335392355646E-17,0.004,0.0068));
#2824=CARTESIAN_POINT('Ctrl Pts',(0.001071796769751,0.004,0.0068));
#2825=CARTESIAN_POINT('Ctrl Pts',(0.00230940107682445,0.004,0.0064427344100728));
#2826=CARTESIAN_POINT('Origin',(0.,0.,0.0068));
#2827=CARTESIAN_POINT('Origin',(0.,0.,0.0068));
#2828=CARTESIAN_POINT('Origin',(0.,0.,0.0068));
#2829=CARTESIAN_POINT('Origin',(0.,0.,0.0068));
#2830=CARTESIAN_POINT('Origin',(0.,0.,0.0068));
#2831=CARTESIAN_POINT('Origin',(0.,0.,0.0068));
#2832=CARTESIAN_POINT('Origin',(0.,0.,0.0068));
#2833=CARTESIAN_POINT('Origin',(0.,0.,0.0068));
#2834=CARTESIAN_POINT('Origin',(0.,0.,0.0068));
#2835=CARTESIAN_POINT('Origin',(0.,0.,0.0068));
#2836=CARTESIAN_POINT('Origin',(0.,0.,0.0068));
#2837=CARTESIAN_POINT('Origin',(0.,0.,0.0068));
#2838=CARTESIAN_POINT('Origin',(-8.67361737988404E-19,-8.67361737988404E-19,
0.0068));
#2839=CARTESIAN_POINT('Origin',(0.,0.,0.000567100162269167));
#2840=CARTESIAN_POINT('',(0.00699395967877932,0.,0.0011));
#2841=CARTESIAN_POINT('',(-0.00699395967877932,-8.56513033398275E-19,0.0011));
#2842=CARTESIAN_POINT('Origin',(0.,0.,0.0011));
#2843=CARTESIAN_POINT('Origin',(0.,0.,0.0011));
#2844=CARTESIAN_POINT('',(-0.0068,-8.327598234202E-19,0.));
#2845=CARTESIAN_POINT('Origin',(-0.0068,-8.327598234202E-19,0.000567100162269167));
#2846=CARTESIAN_POINT('Origin',(0.,0.,0.));
#2847=CARTESIAN_POINT('Origin',(0.,0.,-0.36032464112347));
#2848=CARTESIAN_POINT('',(0.00494387431153844,1.1921208113455E-18,0.00184617005138037));
#2849=CARTESIAN_POINT('',(1.,-1.22464679914735E-16,-0.36032464112347));
#2850=CARTESIAN_POINT('',(0.00247193941718072,-0.00428151672012047,0.00184617090911052));
#2851=CARTESIAN_POINT('Ctrl Pts',(0.00494387431153844,1.1921208113455E-18,
0.00184617005138037));
#2852=CARTESIAN_POINT('Ctrl Pts',(0.00452747332878781,-0.000701807087018258,
0.0019977276146208));
#2853=CARTESIAN_POINT('Ctrl Pts',(0.00368750878396646,-0.00212220560039757,
0.0021900207622692));
#2854=CARTESIAN_POINT('Ctrl Pts',(0.00287197920564823,-0.00356918468363283,
0.00199790178196429));
#2855=CARTESIAN_POINT('Ctrl Pts',(0.00247193941718072,-0.00428151672012047,
0.00184617090911052));
#2856=CARTESIAN_POINT('',(-0.002471932361137,-0.00428152068985298,0.00184617094191608));
#2857=CARTESIAN_POINT('Ctrl Pts',(0.00247193715576922,-0.00428152074690959,
0.00184617005138037));
#2858=CARTESIAN_POINT('Ctrl Pts',(0.00165595444467786,-0.00427181046769567,
0.00199772751317215));
#2859=CARTESIAN_POINT('Ctrl Pts',(5.82745458661851E-6,-0.00425457905249832,
0.00219002124928115));
#2860=CARTESIAN_POINT('Ctrl Pts',(-0.00165501952187246,-0.00427179934699393,
0.00199790093446101));
#2861=CARTESIAN_POINT('Ctrl Pts',(-0.002471932361137,-0.00428152068985298,
0.00184617094191608));
#2862=CARTESIAN_POINT('',(-0.00494387188482622,-4.09000919964499E-9,0.00184617093463073));
#2863=CARTESIAN_POINT('Ctrl Pts',(-0.00247193715576922,-0.00428152074690959,
0.00184617005138037));
#2864=CARTESIAN_POINT('Ctrl Pts',(-0.00287151943030767,-0.00357000337417761,
0.0019977276146208));
#2865=CARTESIAN_POINT('Ctrl Pts',(-0.00368163833127164,-0.00213237352369449,
0.00219002075687879));
#2866=CARTESIAN_POINT('Ctrl Pts',(-0.00452699416225394,-0.000702614689574446,
0.00199790179273536));
#2867=CARTESIAN_POINT('Ctrl Pts',(-0.00494387188482622,-4.09000919964499E-9,
0.00184617093463073));
#2868=CARTESIAN_POINT('',(-0.00247193937985183,0.00428151678659028,0.00184617089495207));
#2869=CARTESIAN_POINT('Ctrl Pts',(-0.00494387431153844,-1.74540774594479E-18,
0.00184617005138037));
#2870=CARTESIAN_POINT('Ctrl Pts',(-0.0045274733287878,0.000701807087018257,
0.0019977276146208));
#2871=CARTESIAN_POINT('Ctrl Pts',(-0.00368750877090321,0.00212220562248781,
0.00219002076525978));
#2872=CARTESIAN_POINT('Ctrl Pts',(-0.00287197918028176,0.00356918472864007,
0.00199790177598857));
#2873=CARTESIAN_POINT('Ctrl Pts',(-0.00247193937985182,0.00428151678659028,
0.00184617089495207));
#2874=CARTESIAN_POINT('',(0.0024719326136737,0.0042815206928582,0.00184617089501096));
#2875=CARTESIAN_POINT('Ctrl Pts',(-0.00247193715576922,0.00428152074690959,
0.00184617005138037));
#2876=CARTESIAN_POINT('Ctrl Pts',(-0.00165595333332649,0.00427181045447048,
0.00199772771959024));
#2877=CARTESIAN_POINT('Ctrl Pts',(-5.91333274921904E-6,0.00425457911567813,
0.00219002026760492));
#2878=CARTESIAN_POINT('Ctrl Pts',(0.00165501039761641,0.00427179923815414,
0.00199790264112614));
#2879=CARTESIAN_POINT('Ctrl Pts',(0.0024719326136737,0.0042815206928582,
0.00184617089501096));
#2880=CARTESIAN_POINT('Ctrl Pts',(0.00247193715576921,0.00428152074690959,
0.00184617005138037));
#2881=CARTESIAN_POINT('Ctrl Pts',(0.00287151943030767,0.0035700033741776,
0.0019977276146208));
#2882=CARTESIAN_POINT('Ctrl Pts',(0.00368163838375097,0.00213237343056514,
0.0021900207693355));
#2883=CARTESIAN_POINT('Ctrl Pts',(0.00452699427177788,0.000702614504335504,
0.00199790176784451));
#2884=CARTESIAN_POINT('Ctrl Pts',(0.00494387204685787,3.81691914936205E-9,
0.00184617087565612));
#2885=CARTESIAN_POINT('Origin',(-8.67361737988404E-19,-8.67361737988404E-19,
0.));
#2886=CARTESIAN_POINT('',(-0.00325,-3.9801020972289E-19,0.));
#2887=CARTESIAN_POINT('Origin',(0.,0.,0.));
#2888=CARTESIAN_POINT('Ctrl Pts',(0.0020802062398655,-0.00439697710233114,
0.00217924420147432));
#2889=CARTESIAN_POINT('Ctrl Pts',(0.00210856163081419,-0.00434786412453955,
0.00188755760062778));
#2890=CARTESIAN_POINT('Ctrl Pts',(0.00236295304044323,-0.00447615069376761,
0.00180329134165063));
#2891=CARTESIAN_POINT('Ctrl Pts',(0.00252613349767768,-0.00362460843532059,
0.00235256917709083));
#2892=CARTESIAN_POINT('Ctrl Pts',(0.002542066495585,-0.00359701167342807,
0.00206498114514791));
#2893=CARTESIAN_POINT('Ctrl Pts',(0.00279156587787958,-0.00371262340768279,
0.00197661181143248));
#2894=CARTESIAN_POINT('Ctrl Pts',(0.00345081170624761,-0.0020230187974257,
0.00258494001506871));
#2895=CARTESIAN_POINT('Ctrl Pts',(0.00345100992757241,-0.00202267546802013,
0.0023096133598543));
#2896=CARTESIAN_POINT('Ctrl Pts',(0.00367050135085753,-0.00214874606333825,
0.0022089697386081));
#2897=CARTESIAN_POINT('Ctrl Pts',(0.00439304074880029,-0.000391030223357476,
0.00235667923254302));
#2898=CARTESIAN_POINT('Ctrl Pts',(0.0043774784205849,-0.000417984966510446,
0.00206916499501039));
#2899=CARTESIAN_POINT('Ctrl Pts',(0.00460190032261363,-0.000576511435992028,
0.00198072177999877));
#2900=CARTESIAN_POINT('Ctrl Pts',(0.00485097725303226,0.000402139068612779,
0.00217804861127444));
#2901=CARTESIAN_POINT('Ctrl Pts',(0.00482257756304232,0.00035294936263097,
0.00188631450420623));
#2902=CARTESIAN_POINT('Ctrl Pts',(0.00506092745585843,0.000196726460696005,
0.00180209579967309));
#2903=CARTESIAN_POINT('Ctrl Pts',(0.00461880215502372,2.60969660665088E-12,
0.00226249222696017));
#2904=CARTESIAN_POINT('Ctrl Pts',(0.00461880493041573,4.80972967263351E-9,
0.00221981071831767));
#2905=CARTESIAN_POINT('Ctrl Pts',(0.00462646565353065,9.25513802947402E-9,
0.00217761263137423));
#2906=CARTESIAN_POINT('Ctrl Pts',(0.00465632814594096,1.66558839052706E-8,
0.00209286153099971));
#2907=CARTESIAN_POINT('Ctrl Pts',(0.00467967919928059,1.93291946404923E-8,
0.00205143483680694));
#2908=CARTESIAN_POINT('Ctrl Pts',(0.00473623848218349,2.17963502552309E-8,
0.00197900347582149));
#2909=CARTESIAN_POINT('Ctrl Pts',(0.00476871684204161,2.16941492436947E-8,
0.00194773373134783));
#2910=CARTESIAN_POINT('Ctrl Pts',(0.00484002106628586,1.99446438725073E-8,
0.00189466116743958));
#2911=CARTESIAN_POINT('Ctrl Pts',(0.00487876012895213,7.20229918431176E-9,
0.00187273694245961));
#2912=CARTESIAN_POINT('Ctrl Pts',(0.00492753919099201,2.65052329180053E-8,
0.00185233276034135));
#2913=CARTESIAN_POINT('Ctrl Pts',(0.0049356821302962,1.06563597029485E-8,
0.00184914982572676));
#2914=CARTESIAN_POINT('Ctrl Pts',(0.00494387279830003,9.92076541137559E-9,
0.00184616902333901));
#2915=CARTESIAN_POINT('Ctrl Pts',(0.00230940107982304,-0.004,0.00226249183548786));
#2916=CARTESIAN_POINT('Ctrl Pts',(0.00230940667748031,-0.00400000000000001,
0.00221981045876485));
#2917=CARTESIAN_POINT('Ctrl Pts',(0.0023132409100976,-0.0040066321208989,
0.00217761250549695));
#2918=CARTESIAN_POINT('Ctrl Pts',(0.00232817856401501,-0.00403248997215914,
0.00209286164541814));
#2919=CARTESIAN_POINT('Ctrl Pts',(0.00233985638039947,-0.00405271115271212,
0.00205143505643002));
#2920=CARTESIAN_POINT('Ctrl Pts',(0.00236813813045257,-0.00410169160548647,
0.0019790036952096));
#2921=CARTESIAN_POINT('Ctrl Pts',(0.0023843772427971,-0.00412981877908601,
0.00194773388444953));
#2922=CARTESIAN_POINT('Ctrl Pts',(0.00242002790301579,-0.00419157106220532,
0.00189466118804628));
#2923=CARTESIAN_POINT('Ctrl Pts',(0.00243938639823226,-0.00422512665324962,
0.00187273688517089));
#2924=CARTESIAN_POINT('Ctrl Pts',(0.00246379267336123,-0.00426736064254826,
0.00185233281178718));
#2925=CARTESIAN_POINT('Ctrl Pts',(0.00246785033449192,-0.00427442067365005,
0.00184914985094565));
#2926=CARTESIAN_POINT('Ctrl Pts',(0.00247194491204864,-0.00428151417461562,
0.00184616912670582));
#2927=CARTESIAN_POINT('Ctrl Pts',(-0.00276909135727935,-0.004,0.00217899169790385));
#2928=CARTESIAN_POINT('Ctrl Pts',(-0.00271235704649767,-0.00399999999999999,
0.00188729521822938));
#2929=CARTESIAN_POINT('Ctrl Pts',(-0.00269626039969526,-0.00428446969999985,
0.00180303837461786));
#2930=CARTESIAN_POINT('Ctrl Pts',(-0.00187685966992971,-0.004,0.00235244886375929));
#2931=CARTESIAN_POINT('Ctrl Pts',(-0.00184499447367401,-0.00400000000000006,
0.00206485113824212));
#2932=CARTESIAN_POINT('Ctrl Pts',(-0.00182033920767984,-0.00427389079720739,
0.00197649100614117));
#2933=CARTESIAN_POINT('Ctrl Pts',(-2.68059993290473E-5,-0.004,0.00258505308205348));
#2934=CARTESIAN_POINT('Ctrl Pts',(-2.64037614343951E-5,-0.00399999999999977,
0.00230972896816672));
#2935=CARTESIAN_POINT('Ctrl Pts',(-2.58366266104264E-5,-0.00425311179830988,
0.00220908222014014));
#2936=CARTESIAN_POINT('Ctrl Pts',(0.00185878890297778,-0.004,0.00235657272456735));
#2937=CARTESIAN_POINT('Ctrl Pts',(0.00182766695568966,-0.00400000000000039,
0.00206904911217261));
#2938=CARTESIAN_POINT('Ctrl Pts',(0.00180255912815774,-0.00427362955430766,
0.00198061477916247));
#2939=CARTESIAN_POINT('Ctrl Pts',(0.00277510174796861,-0.004,0.00217778485182945));
#2940=CARTESIAN_POINT('Ctrl Pts',(0.00271827814865782,-0.00399999999999991,
0.00188604038028264));
#2941=CARTESIAN_POINT('Ctrl Pts',(0.00270215958680058,-0.00428454621889335,
0.00180183157755754));
#2942=CARTESIAN_POINT('Ctrl Pts',(-0.00230940107522602,-0.00400000000265434,
0.00226249222695167));
#2943=CARTESIAN_POINT('Ctrl Pts',(-0.00230939827617001,-0.00400000485076157,
0.0022198103539442));
#2944=CARTESIAN_POINT('Ctrl Pts',(-0.00231322483018635,-0.00400664160220837,
0.00217761191602451));
#2945=CARTESIAN_POINT('Ctrl Pts',(-0.00232814975025645,-0.00403250724714706,
0.00209286083905841));
#2946=CARTESIAN_POINT('Ctrl Pts',(-0.00233982289833555,-0.00405273112360759,
0.00205143444336701));
#2947=CARTESIAN_POINT('Ctrl Pts',(-0.00236810006107592,-0.0041017135810827,
0.00197900396916589));
#2948=CARTESIAN_POINT('Ctrl Pts',(-0.00238433899975335,-0.00412984004164373,
0.00194773472029215));
#2949=CARTESIAN_POINT('Ctrl Pts',(-0.0024199904598784,-0.00419158665219816,
0.00189466492377884));
#2950=CARTESIAN_POINT('Ctrl Pts',(-0.00243936900505325,-0.00422512562446801,
0.00187274224654465));
#2951=CARTESIAN_POINT('Ctrl Pts',(-0.00246374483466011,-0.00426738465712574,
0.00185233386579348));
#2952=CARTESIAN_POINT('Ctrl Pts',(-0.00246782572589702,-0.00427442103508152,
0.00184915496726748));
#2953=CARTESIAN_POINT('Ctrl Pts',(-0.00247192721594409,-0.00428152353602606,
0.00184617013594552));
#2954=CARTESIAN_POINT('Ctrl Pts',(0.00484799699036367,-0.000396977102250874,
0.00217924420149234));
#2955=CARTESIAN_POINT('Ctrl Pts',(0.0048196415994154,-0.000347864124460288,
0.00188755760064398));
#2956=CARTESIAN_POINT('Ctrl Pts',(0.00505793673214804,-0.000191697985830489,
0.00180329134166766));
#2957=CARTESIAN_POINT('Ctrl Pts',(0.00440206973256443,0.000375391564737258,
0.00235256917709936));
#2958=CARTESIAN_POINT('Ctrl Pts',(0.00438613673465794,0.00040298832662938,
0.00206498114515469));
#2959=CARTESIAN_POINT('Ctrl Pts',(0.00461100912464618,0.000561255262797908,
0.00197661181144046));
#2960=CARTESIAN_POINT('Ctrl Pts',(0.0034773915240279,0.00197698120257433,
0.00258494001506013));
#2961=CARTESIAN_POINT('Ctrl Pts',(0.00347719330270246,0.00197732453198037,
0.0023096133598436));
#2962=CARTESIAN_POINT('Ctrl Pts',(0.00369611935256539,0.00210437438280086,
0.00220896973859817));
#2963=CARTESIAN_POINT('Ctrl Pts',(0.00253516248150867,0.00360896977658459,
0.00235667923255163));
#2964=CARTESIAN_POINT('Ctrl Pts',(0.00255072480972449,0.00358201503343101,
0.00206916499501691));
#2965=CARTESIAN_POINT('Ctrl Pts',(0.00280022371048194,0.00369710686701457,
0.00198072178000659));
#2966=CARTESIAN_POINT('Ctrl Pts',(0.002077225977291,0.00440213906853008,
0.00217804861129297));
#2967=CARTESIAN_POINT('Ctrl Pts',(0.00210562566728017,0.00435294936254953,
0.00188631450422304));
#2968=CARTESIAN_POINT('Ctrl Pts',(0.00236009361541863,0.00448125497375149,
0.00180209579969069));
#2969=CARTESIAN_POINT('Ctrl Pts',(0.0023094010752774,0.00400000000256537,
0.00226249222696888));
#2970=CARTESIAN_POINT('Ctrl Pts',(0.0023093983235636,0.00400000476867347,
0.00221981080901497));
#2971=CARTESIAN_POINT('Ctrl Pts',(0.00231322484200826,0.0040066413091479,
0.00217761280825381));
#2972=CARTESIAN_POINT('Ctrl Pts',(0.00232814966084154,0.00403250653132782,
0.00209286186351978));
#2973=CARTESIAN_POINT('Ctrl Pts',(0.0023398228431364,0.00405273037837203,
0.00205143523833409));
#2974=CARTESIAN_POINT('Ctrl Pts',(0.00236810032719515,0.0041017133110918,
0.00197900379862345));
#2975=CARTESIAN_POINT('Ctrl Pts',(0.00238433962881604,0.00412984040412892,
0.00194773394920763));
#2976=CARTESIAN_POINT('Ctrl Pts',(0.00241999332152723,0.00419159094343347,
0.00189466123632128));
#2977=CARTESIAN_POINT('Ctrl Pts',(0.00243937381272943,0.00422513365863828,
0.00187273698229547));
#2978=CARTESIAN_POINT('Ctrl Pts',(0.00246374684853763,0.00426738730103737,
0.00185233273837006));
#2979=CARTESIAN_POINT('Ctrl Pts',(0.00246783178595212,0.00427443117503508,
0.00184914992183635));
#2980=CARTESIAN_POINT('Ctrl Pts',(0.00247192773993968,0.00428152411588965,
0.00184616912415846));
#2981=CARTESIAN_POINT('Ctrl Pts',(-0.00484799699031254,0.000396977102162332,
0.00217924420151239));
#2982=CARTESIAN_POINT('Ctrl Pts',(-0.00481964159936525,0.000347864124373369,
0.00188755760066478));
#2983=CARTESIAN_POINT('Ctrl Pts',(-0.00505793673209653,0.000191697985744254,
0.00180329134168764));
#2984=CARTESIAN_POINT('Ctrl Pts',(-0.00440206973252995,-0.000375391564796995,
0.00235256917710718));
#2985=CARTESIAN_POINT('Ctrl Pts',(-0.00438613673462329,-0.000402988326689221,
0.00206498114516339));
#2986=CARTESIAN_POINT('Ctrl Pts',(-0.00461100912461266,-0.000561255262855402,
0.0019766118114488));
#2987=CARTESIAN_POINT('Ctrl Pts',(-0.00347739152402765,-0.00197698120257474,
0.0025849400150519));
#2988=CARTESIAN_POINT('Ctrl Pts',(-0.00347719330270223,-0.00197732453198073,
0.00230961335983513));
#2989=CARTESIAN_POINT('Ctrl Pts',(-0.00369611935256536,-0.00210437438280157,
0.0022089697385899));
#2990=CARTESIAN_POINT('Ctrl Pts',(-0.00253516248154363,-0.00360896977652404,
0.00235667923256029));
#2991=CARTESIAN_POINT('Ctrl Pts',(-0.00255072480975946,-0.00358201503337074,
0.00206916499502631));
#2992=CARTESIAN_POINT('Ctrl Pts',(-0.00280022371051508,-0.00369710686695539,
0.00198072178001496));
#2993=CARTESIAN_POINT('Ctrl Pts',(-0.00207722597734354,-0.00440213906843907,
0.00217804861131337));
#2994=CARTESIAN_POINT('Ctrl Pts',(-0.0021056256673318,-0.00435294936246005,
0.00188631450424426));
#2995=CARTESIAN_POINT('Ctrl Pts',(-0.00236009361546901,-0.00448125497366147,
0.00180209579971121));
#2996=CARTESIAN_POINT('Ctrl Pts',(-0.00461880215502371,-2.60969740465829E-12,
0.00226249222696032));
#2997=CARTESIAN_POINT('Ctrl Pts',(-0.00461880493044008,-4.80977186674728E-9,
0.00221981034336869));
#2998=CARTESIAN_POINT('Ctrl Pts',(-0.00462646578784855,-9.25521530506121E-9,
0.00217761189364838));
#2999=CARTESIAN_POINT('Ctrl Pts',(-0.00465632853642066,-1.66559319787286E-8,
0.00209286081607735));
#3000=CARTESIAN_POINT('Ctrl Pts',(-0.00467967949048832,-1.93292113464515E-8,
0.00205143443431073));
#3001=CARTESIAN_POINT('Ctrl Pts',(-0.00473623815244463,-2.17963318402135E-8,
0.00197900392609519));
#3002=CARTESIAN_POINT('Ctrl Pts',(-0.00476871590488861,-2.16941546676782E-8,
0.0019477346444674));
#3003=CARTESIAN_POINT('Ctrl Pts',(-0.00484001587792066,-1.99447883239839E-8,
0.00189466481646245));
#3004=CARTESIAN_POINT('Ctrl Pts',(-0.0048787507470625,-7.2202173171277E-9,
0.00187274215724451));
#3005=CARTESIAN_POINT('Ctrl Pts',(-0.00492753617461704,-2.64997623468435E-8,
0.00185233376728398));
#3006=CARTESIAN_POINT('Ctrl Pts',(-0.00493567013491418,-1.06587769589897E-8,
0.0018491549351575));
#3007=CARTESIAN_POINT('Ctrl Pts',(-0.00494387177388727,-9.92086063382213E-9,
0.00184617012407515));
#3008=CARTESIAN_POINT('Ctrl Pts',(0.00276648183574491,0.004,0.00217949823698557));
#3009=CARTESIAN_POINT('Ctrl Pts',(0.00270979471839317,0.00399999999999989,
0.00188782157682243));
#3010=CARTESIAN_POINT('Ctrl Pts',(0.00269369884333924,0.00428443560947813,
0.00180354584308321));
#3011=CARTESIAN_POINT('Ctrl Pts',(0.00187500692923374,0.004,0.00235269014572225));
#3012=CARTESIAN_POINT('Ctrl Pts',(0.00184314015037907,0.00400000000000045,
0.00206511185901196));
#3013=CARTESIAN_POINT('Ctrl Pts',(0.00181854159277439,0.0042738664773099,
0.00197673327463295));
#3014=CARTESIAN_POINT('Ctrl Pts',(2.63535568577022E-5,0.004,0.00258482628539704));
#3015=CARTESIAN_POINT('Ctrl Pts',(2.59629106265878E-5,0.00399999999999955,
0.00230949707126385));
#3016=CARTESIAN_POINT('Ctrl Pts',(2.53992995043738E-5,0.00425312914551421,
0.00220885659731835));
#3017=CARTESIAN_POINT('Ctrl Pts',(-0.00185696196096345,0.004,0.00235678640664226));
#3018=CARTESIAN_POINT('Ctrl Pts',(-0.00182583461132829,0.0040000000000005,
0.00206928159589147));
#3019=CARTESIAN_POINT('Ctrl Pts',(-0.00180078859598649,0.00427360698479904,
0.00198082944956426));
#3020=CARTESIAN_POINT('Ctrl Pts',(-0.00277239243853729,0.004,0.00217831389249534));
#3021=CARTESIAN_POINT('Ctrl Pts',(-0.00271561741455655,0.00399999999999988,
0.00188659021085909));
#3022=CARTESIAN_POINT('Ctrl Pts',(-0.00269949989932968,0.00428451070179002,
0.00180236154602939));
#3023=CARTESIAN_POINT('Ctrl Pts',(-0.00230940107972112,0.004,0.00226249261916749));
#3024=CARTESIAN_POINT('Ctrl Pts',(-0.00230940658357872,0.00400000000000002,
0.00221981070558142));
#3025=CARTESIAN_POINT('Ctrl Pts',(-0.00231324082258085,0.00400663228001755,
0.0021776122207903));
#3026=CARTESIAN_POINT('Ctrl Pts',(-0.00232817854337327,0.0040324904929674,
0.00209286106268009));
#3027=CARTESIAN_POINT('Ctrl Pts',(-0.00233985631668495,0.00405271168730321,
0.00205143463328512));
#3028=CARTESIAN_POINT('Ctrl Pts',(-0.00236813776484925,0.00410169169915766,
0.00197900406377293));
#3029=CARTESIAN_POINT('Ctrl Pts',(-0.00238437654793324,0.00412981829929945,
0.00194773476157516));
#3030=CARTESIAN_POINT('Ctrl Pts',(-0.00242002502086811,0.00419156673501641,
0.00189466489996567));
#3031=CARTESIAN_POINT('Ctrl Pts',(-0.00243938148784039,0.00422511835941925,
0.00187274224703594));
#3032=CARTESIAN_POINT('Ctrl Pts',(-0.00246379100631313,0.00426735863971814,
0.00185233363819034));
#3033=CARTESIAN_POINT('Ctrl Pts',(-0.00246784451355287,0.00427441094564068,
0.00184915470496365));
#3034=CARTESIAN_POINT('Ctrl Pts',(-0.00247194489770891,0.00428151448007287,
0.00184616976692702));
#3035=CARTESIAN_POINT('Ctrl Pts',(-0.00208020623988541,0.00439697710229665,
0.00217924420148206));
#3036=CARTESIAN_POINT('Ctrl Pts',(-0.00210856163083422,0.00434786412450488,
0.00188755760063093));
#3037=CARTESIAN_POINT('Ctrl Pts',(-0.00236295304046781,0.00447615069373628,
0.00180329134165656));
#3038=CARTESIAN_POINT('Ctrl Pts',(-0.00252613349769144,0.00362460843529674,
0.0023525691770943));
#3039=CARTESIAN_POINT('Ctrl Pts',(-0.00254206649559906,0.00359701167340373,
0.0020649811451469));
#3040=CARTESIAN_POINT('Ctrl Pts',(-0.00279156587789806,0.00371262340766202,
0.00197661181143402));
#3041=CARTESIAN_POINT('Ctrl Pts',(-0.00345081170624774,0.00202301879742548,
0.00258494001506496));
#3042=CARTESIAN_POINT('Ctrl Pts',(-0.00345100992757254,0.00202267546801992,
0.00230961335984592));
#3043=CARTESIAN_POINT('Ctrl Pts',(-0.00367050135086289,0.00214874606334101,
0.00220896973860242));
#3044=CARTESIAN_POINT('Ctrl Pts',(-0.00439304074878628,0.000391030223381733,
0.00235667923254706));
#3045=CARTESIAN_POINT('Ctrl Pts',(-0.00437747842057059,0.000417984966535182,
0.00206916499501008));
#3046=CARTESIAN_POINT('Ctrl Pts',(-0.00460190032260445,0.000576511436018824,
0.00198072178000032));
#3047=CARTESIAN_POINT('Ctrl Pts',(-0.0048509772530118,-0.000402139068577363,
0.00217804861128226));
#3048=CARTESIAN_POINT('Ctrl Pts',(-0.00482257756302177,-0.000352949362595358,
0.00188631450420942));
#3049=CARTESIAN_POINT('Ctrl Pts',(-0.0050609274558431,-0.000196726460658123,
0.00180209579967924));
#3050=CARTESIAN_POINT('Origin',(0.,0.,-0.025));
#3051=CARTESIAN_POINT('',(-0.003,-3.67394039744206E-19,-0.000249999999999999));
#3052=CARTESIAN_POINT('Origin',(0.,0.,-0.00025));
#3053=CARTESIAN_POINT('',(-0.003,0.,-0.024458734125));
#3054=CARTESIAN_POINT('',(-0.003,-3.67394039744206E-19,-0.025));
#3055=CARTESIAN_POINT('Origin',(0.,0.,-0.024458734125));
#3056=CARTESIAN_POINT('Origin',(0.,0.,-0.025));
#3057=CARTESIAN_POINT('',(-0.002458734125,0.,-0.025));
#3058=CARTESIAN_POINT('Origin',(0.,0.,-0.025));
#3059=CARTESIAN_POINT('Origin',(0.,0.,-0.00025));
#3060=CARTESIAN_POINT('Origin',(-0.00325,-3.9801020972289E-19,-0.00025));
#3061=CARTESIAN_POINT('Origin',(0.,0.,-0.025));
#3062=CARTESIAN_POINT('',(-0.002458734125,-3.01108087613562E-19,-0.025));
#3063=CARTESIAN_POINT('',(0.,0.,0.));
#3064=CARTESIAN_POINT('Origin',(0.,0.005,0.003));
#3065=CARTESIAN_POINT('',(0.00288675134594812,0.005,0.0025534180126148));
#3066=CARTESIAN_POINT('',(0.00288675134594812,0.005,-0.00125469561686031));
#3067=CARTESIAN_POINT('',(0.00288675134594812,0.005,0.003));
#3068=CARTESIAN_POINT('',(-0.00288674534909874,0.00499999549622412,-0.0012546876068247));
#3069=CARTESIAN_POINT('Ctrl Pts',(0.00288674086811144,0.005,-0.00125466832470784));
#3070=CARTESIAN_POINT('Ctrl Pts',(0.00240905318327833,0.005,-0.00117291044573697));
#3071=CARTESIAN_POINT('Ctrl Pts',(0.00192881231229982,0.00499999999750974,
-0.00110698869329289));
#3072=CARTESIAN_POINT('Ctrl Pts',(0.00144725210385079,0.00500000000251777,
-0.0010616014875037));
#3073=CARTESIAN_POINT('Ctrl Pts',(0.000972923765006934,0.00500000000745059,
-0.00101689588776968));
#3074=CARTESIAN_POINT('Ctrl Pts',(0.000497315857174576,0.00500000004285957,
-0.00099213963141374));
#3075=CARTESIAN_POINT('Ctrl Pts',(2.17100169132483E-5,0.00500000001549357,
-0.000991518738265624));
#3076=CARTESIAN_POINT('Ctrl Pts',(1.44586698218705E-5,0.00500000001507633,
-0.000991509271788676));
#3077=CARTESIAN_POINT('Ctrl Pts',(7.20731733020144E-6,0.00500000001465332,
-0.000991505417348841));
#3078=CARTESIAN_POINT('Ctrl Pts',(-4.40332323880218E-8,0.00500000001422604,
-0.000991507156144612));
#3079=CARTESIAN_POINT('Ctrl Pts',(-0.000482901451728483,0.00499999998577425,
-0.000991622940153412));
#3080=CARTESIAN_POINT('Ctrl Pts',(-0.000965714799268779,0.005,-0.00101680380767097));
#3081=CARTESIAN_POINT('Ctrl Pts',(-0.00144724102982738,0.005,-0.00106216147680642));
#3082=CARTESIAN_POINT('Ctrl Pts',(-0.00192876726038598,0.005,-0.00110751914594187));
#3083=CARTESIAN_POINT('Ctrl Pts',(-0.00240902863327068,0.005,-0.00117307891969936));
#3084=CARTESIAN_POINT('Ctrl Pts',(-0.00288673415173692,0.005,-0.00125470733476186));
#3085=CARTESIAN_POINT('',(-0.00288675134594812,0.005,0.0025534180126148));
#3086=CARTESIAN_POINT('',(-0.00288675134594813,0.005,0.003));
#3087=CARTESIAN_POINT('',(0.,0.005,0.003));
#3088=CARTESIAN_POINT('Ctrl Pts',(-0.00288675134596021,0.005,0.00255341801261131));
#3089=CARTESIAN_POINT('Ctrl Pts',(-0.00133974596216047,0.005,0.003));
#3090=CARTESIAN_POINT('Ctrl Pts',(0.,0.005,0.003));
#3091=CARTESIAN_POINT('Ctrl Pts',(0.,0.005,0.003));
#3092=CARTESIAN_POINT('Ctrl Pts',(0.00133974596216047,0.005,0.003));
#3093=CARTESIAN_POINT('Ctrl Pts',(0.0028867513459602,0.005,0.00255341801261131));
#3094=CARTESIAN_POINT('Origin',(-0.00433012701892219,0.0025,0.003));
#3095=CARTESIAN_POINT('',(-0.00577349577362417,2.97524700789561E-9,-0.00125468783280795));
#3096=CARTESIAN_POINT('Ctrl Pts',(-0.00288675654646056,0.00499999099244825,
-0.00125466787888755));
#3097=CARTESIAN_POINT('Ctrl Pts',(-0.00312559936895968,0.00458630308885661,
-0.00117290882464078));
#3098=CARTESIAN_POINT('Ctrl Pts',(-0.00336571418606295,0.00417041202041243,
-0.001106984526675));
#3099=CARTESIAN_POINT('Ctrl Pts',(-0.00360648916145778,0.00375337754104142,
-0.00106159956055554));
#3100=CARTESIAN_POINT('Ctrl Pts',(-0.00384362185895275,0.00334265167187877,
-0.0010169011469269));
#3101=CARTESIAN_POINT('Ctrl Pts',(-0.00408139429007746,0.00293081781202513,
-0.000992145259800431));
#3102=CARTESIAN_POINT('Ctrl Pts',(-0.00431917052189825,0.00251897724138379,
-0.000991520603317846));
#3103=CARTESIAN_POINT('Ctrl Pts',(-0.00432282268426734,0.00251265150973835,
-0.000991511008805889));
#3104=CARTESIAN_POINT('Ctrl Pts',(-0.00432647485050128,0.00250632577138726,
-0.000991507108821008));
#3105=CARTESIAN_POINT('Ctrl Pts',(-0.00433012701679626,0.00250000003292203,
-0.00099150888414755));
#3106=CARTESIAN_POINT('Ctrl Pts',(-0.00457155567050904,0.00208183327980953,
-0.000991626243178409));
#3107=CARTESIAN_POINT('Ctrl Pts',(-0.00481296724285258,0.00166369620021464,
-0.00101680902829736));
#3108=CARTESIAN_POINT('Ctrl Pts',(-0.00505373559306525,0.00124667318479177,
-0.00106216623675387));
#3109=CARTESIAN_POINT('Ctrl Pts',(-0.00529450394327791,0.000829650169368897,
-0.00110752344521038));
#3110=CARTESIAN_POINT('Ctrl Pts',(-0.00553464028677118,0.000413721821694746,
-0.00117308056855006));
#3111=CARTESIAN_POINT('Ctrl Pts',(-0.00577349405586451,1.49580457720067E-8,
-0.00125470778672834));
#3112=CARTESIAN_POINT('',(-0.00577350269189626,-1.7347234759768E-18,0.0025534180126148));
#3113=CARTESIAN_POINT('',(-0.00577350269189626,4.33680868994202E-19,0.003));
#3114=CARTESIAN_POINT('',(-0.00433012701892219,0.0025,0.003));
#3115=CARTESIAN_POINT('Ctrl Pts',(-0.0057735026919023,-1.04763274033972E-14,
0.00255341801261131));
#3116=CARTESIAN_POINT('Ctrl Pts',(-0.00500000000000243,0.0013397459621514,
0.003));
#3117=CARTESIAN_POINT('Ctrl Pts',(-0.00433012701892219,0.0025,0.003));
#3118=CARTESIAN_POINT('Ctrl Pts',(-0.00433012701892219,0.0025,0.003));
#3119=CARTESIAN_POINT('Ctrl Pts',(-0.00366025403784195,0.0036602540378486,
0.003));
#3120=CARTESIAN_POINT('Ctrl Pts',(-0.00288675134594208,0.00500000000001047,
0.00255341801261131));
#3121=CARTESIAN_POINT('Origin',(-0.00433012701892219,-0.0025,0.003));
#3122=CARTESIAN_POINT('',(-0.00288675049891667,-0.0049999925209771,-0.00125468762698494));
#3123=CARTESIAN_POINT('Ctrl Pts',(-0.00577349749138383,-9.00755175621548E-9,
-0.00125466787888756));
#3124=CARTESIAN_POINT('Ctrl Pts',(-0.00553465466888472,-0.000413696911143376,
-0.00117290882464071));
#3125=CARTESIAN_POINT('Ctrl Pts',(-0.00529453984695666,-0.000829587976801908,
-0.00110698452667449));
#3126=CARTESIAN_POINT('Ctrl Pts',(-0.00505376488126475,-0.00124662246177494,
-0.00106159956055528));
#3127=CARTESIAN_POINT('Ctrl Pts',(-0.00481663219332592,-0.00165734833645486,
-0.00101690114692689));
#3128=CARTESIAN_POINT('Ctrl Pts',(-0.00457885982411642,-0.00206918223205526,
-0.000992145259800429));
#3129=CARTESIAN_POINT('Ctrl Pts',(-0.00434108354354234,-0.00248102277454885,
-0.000991520603318092));
#3130=CARTESIAN_POINT('Ctrl Pts',(-0.00433743138042441,-0.00248734850576196,
-0.000991511008806138));
#3131=CARTESIAN_POINT('Ctrl Pts',(-0.00433377921343164,-0.00249367424367495,
-0.00099150710882126));
#3132=CARTESIAN_POINT('Ctrl Pts',(-0.00433012704637054,-0.00249999998169787,
-0.000991508884147806));
#3133=CARTESIAN_POINT('Ctrl Pts',(-0.00408869834201345,-0.00291816670557085,
-0.000991626243178921));
#3134=CARTESIAN_POINT('Ctrl Pts',(-0.00384728679499185,-0.00333630379978529,
-0.00101680902829835));
#3135=CARTESIAN_POINT('Ctrl Pts',(-0.00360651844477919,-0.00375332681520815,
-0.00106216623675482));
#3136=CARTESIAN_POINT('Ctrl Pts',(-0.00336575009456654,-0.004170349830631,
-0.00110752344521128));
#3137=CARTESIAN_POINT('Ctrl Pts',(-0.00312561375107325,-0.0045862781783052,
-0.00117308056855045));
#3138=CARTESIAN_POINT('Ctrl Pts',(-0.0028867599819799,-0.00499998504195421,
-0.00125470778672846));
#3139=CARTESIAN_POINT('',(-0.00288675134594813,-0.005,0.0025534180126148));
#3140=CARTESIAN_POINT('',(-0.00288675134594812,-0.005,0.003));
#3141=CARTESIAN_POINT('',(-0.00433012701892219,-0.0025,0.003));
#3142=CARTESIAN_POINT('Ctrl Pts',(-0.00288675134594208,-0.00500000000001047,
0.00255341801261131));
#3143=CARTESIAN_POINT('Ctrl Pts',(-0.00366025403784195,-0.0036602540378486,
0.003));
#3144=CARTESIAN_POINT('Ctrl Pts',(-0.00433012701892219,-0.0025,0.003));
#3145=CARTESIAN_POINT('Ctrl Pts',(-0.00433012701892219,-0.0025,0.003));
#3146=CARTESIAN_POINT('Ctrl Pts',(-0.00500000000000243,-0.0013397459621514,
0.003));
#3147=CARTESIAN_POINT('Ctrl Pts',(-0.0057735026919023,1.04765720059514E-14,
0.00255341801261131));
#3148=CARTESIAN_POINT('Origin',(2.60208521396521E-18,-0.005,0.003));
#3149=CARTESIAN_POINT('',(0.00288674527580217,-0.00499999549622412,-0.00125468803234519));
#3150=CARTESIAN_POINT('Ctrl Pts',(-0.00288674101585344,-0.005,-0.00125466746724142));
#3151=CARTESIAN_POINT('Ctrl Pts',(-0.00240905736903686,-0.005,-0.00117290734672732));
#3152=CARTESIAN_POINT('Ctrl Pts',(-0.00192883892611274,-0.00499999999694111,
-0.0011069808211488));
#3153=CARTESIAN_POINT('Ctrl Pts',(-0.00144729928597653,-0.00500000000309269,
-0.00106159786290637));
#3154=CARTESIAN_POINT('Ctrl Pts',(-0.000973082182196052,-0.00500000000915072,
-0.00101690502097829));
#3155=CARTESIAN_POINT('Ctrl Pts',(-0.000497585721015049,-0.00500000004512902,
-0.000992149362934236));
#3156=CARTESIAN_POINT('Ctrl Pts',(-2.20717975660666E-5,-0.00500000001630823,
-0.00099152216154249));
#3157=CARTESIAN_POINT('Ctrl Pts',(-1.47292366074848E-5,-0.0050000000158632,
-0.000991512476727336));
#3158=CARTESIAN_POINT('Ctrl Pts',(-7.3866655541157E-6,-0.00500000001541243,
-0.000991508546376759));
#3159=CARTESIAN_POINT('Ctrl Pts',(-4.4092249370988E-8,-0.00500000001495753,
-0.000991510350975005));
#3160=CARTESIAN_POINT('Ctrl Pts',(0.000482813204058313,-0.00499999998504277,
-0.000991629023733715));
#3161=CARTESIAN_POINT('Ctrl Pts',(0.000965646141812395,-0.005,-0.00101681337172211));
#3162=CARTESIAN_POINT('Ctrl Pts',(0.00144719332304809,-0.005,-0.0010621702020272));
#3163=CARTESIAN_POINT('Ctrl Pts',(0.00192874050428379,-0.005,-0.00110752703233228));
#3164=CARTESIAN_POINT('Ctrl Pts',(0.00240902445338621,-0.005,-0.00117308198576979));
#3165=CARTESIAN_POINT('Ctrl Pts',(0.00288673400514377,-0.005,-0.00125470818580277));
#3166=CARTESIAN_POINT('',(0.00288675134594813,-0.005,0.0025534180126148));
#3167=CARTESIAN_POINT('',(0.00288675134594813,-0.005,0.003));
#3168=CARTESIAN_POINT('',(0.,-0.005,0.003));
#3169=CARTESIAN_POINT('Ctrl Pts',(-6.35714439048776E-18,-0.005,0.003));
#3170=CARTESIAN_POINT('Ctrl Pts',(0.00133974596216047,-0.005,0.003));
#3171=CARTESIAN_POINT('Ctrl Pts',(0.00288675134596023,-0.005,0.00255341801261131));
#3172=CARTESIAN_POINT('Ctrl Pts',(-0.00288675134596022,-0.005,0.00255341801261131));
#3173=CARTESIAN_POINT('Ctrl Pts',(-0.00133974596216048,-0.005,0.003));
#3174=CARTESIAN_POINT('Ctrl Pts',(-6.35714439048776E-18,-0.005,0.003));
#3175=CARTESIAN_POINT('Origin',(0.00433012701892219,-0.0025,0.003));
#3176=CARTESIAN_POINT('',(0.00577349577362418,-2.97524702184282E-9,-0.00125468783280786));
#3177=CARTESIAN_POINT('Ctrl Pts',(0.00288675654646057,-0.00499999099244824,
-0.00125466787888762));
#3178=CARTESIAN_POINT('Ctrl Pts',(0.0031255993689597,-0.00458630308885659,
-0.00117290882464094));
#3179=CARTESIAN_POINT('Ctrl Pts',(0.00336571418606296,-0.00417041202041241,
-0.00110698452667517));
#3180=CARTESIAN_POINT('Ctrl Pts',(0.00360648916145779,-0.00375337754104141,
-0.00106159956055563));
#3181=CARTESIAN_POINT('Ctrl Pts',(0.00384362185895275,-0.00334265167187877,
-0.0010169011469269));
#3182=CARTESIAN_POINT('Ctrl Pts',(0.00408139429007746,-0.00293081781202513,
-0.000992145259800431));
#3183=CARTESIAN_POINT('Ctrl Pts',(0.00431917052189824,-0.0025189772413838,
-0.000991520603317827));
#3184=CARTESIAN_POINT('Ctrl Pts',(0.00432282268426734,-0.00251265150973835,
-0.00099151100880587));
#3185=CARTESIAN_POINT('Ctrl Pts',(0.00432647485050128,-0.00250632577138726,
-0.000991507108820988));
#3186=CARTESIAN_POINT('Ctrl Pts',(0.00433012701679626,-0.00250000003292203,
-0.00099150888414753));
#3187=CARTESIAN_POINT('Ctrl Pts',(0.00457155567050903,-0.00208183327980953,
-0.00099162624317837));
#3188=CARTESIAN_POINT('Ctrl Pts',(0.00481296724285258,-0.00166369620021464,
-0.00101680902829732));
#3189=CARTESIAN_POINT('Ctrl Pts',(0.00505373559306524,-0.00124667318479177,
-0.00106216623675383));
#3190=CARTESIAN_POINT('Ctrl Pts',(0.00529450394327791,-0.000829650169368892,
-0.00110752344521035));
#3191=CARTESIAN_POINT('Ctrl Pts',(0.00553464028677118,-0.00041372182169474,
-0.00117308056855006));
#3192=CARTESIAN_POINT('Ctrl Pts',(0.00577349405586451,-1.4958045768121E-8,
-0.00125470778672835));
#3193=CARTESIAN_POINT('',(0.00577350269189626,2.60208521396521E-18,0.0025534180126148));
#3194=CARTESIAN_POINT('',(0.00577350269189626,2.60208521396521E-18,0.003));
#3195=CARTESIAN_POINT('',(0.00433012701892219,-0.0025,0.003));
#3196=CARTESIAN_POINT('Ctrl Pts',(0.00577350269190231,1.04782842238321E-14,
0.00255341801261131));
#3197=CARTESIAN_POINT('Ctrl Pts',(0.00500000000000243,-0.0013397459621514,
0.003));
#3198=CARTESIAN_POINT('Ctrl Pts',(0.00433012701892219,-0.0025,0.003));
#3199=CARTESIAN_POINT('Ctrl Pts',(0.00433012701892219,-0.0025,0.003));
#3200=CARTESIAN_POINT('Ctrl Pts',(0.00366025403784196,-0.0036602540378486,
0.003));
#3201=CARTESIAN_POINT('Ctrl Pts',(0.00288675134594208,-0.00500000000001048,
0.00255341801261131));
#3202=CARTESIAN_POINT('Origin',(0.00433012701892219,0.0025,0.003));
#3203=CARTESIAN_POINT('Ctrl Pts',(0.00577349749138385,9.00755172443538E-9,
-0.00125466787888738));
#3204=CARTESIAN_POINT('Ctrl Pts',(0.00553465466888475,0.000413696911143324,
-0.00117290882464032));
#3205=CARTESIAN_POINT('Ctrl Pts',(0.00529453984695666,0.000829587976801907,
-0.00110698452667446));
#3206=CARTESIAN_POINT('Ctrl Pts',(0.00505376488126474,0.00124662246177494,
-0.00106159956055527));
#3207=CARTESIAN_POINT('Ctrl Pts',(0.00481663219332591,0.00165734833645487,
-0.00101690114692689));
#3208=CARTESIAN_POINT('Ctrl Pts',(0.00457885982411642,0.00206918223205527,
-0.000992145259800432));
#3209=CARTESIAN_POINT('Ctrl Pts',(0.00434108354354234,0.00248102277454886,
-0.000991520603317914));
#3210=CARTESIAN_POINT('Ctrl Pts',(0.00433743138042441,0.00248734850576197,
-0.000991511008805958));
#3211=CARTESIAN_POINT('Ctrl Pts',(0.00433377921343164,0.00249367424367496,
-0.000991507108821077));
#3212=CARTESIAN_POINT('Ctrl Pts',(0.00433012704637054,0.00249999998169787,
-0.00099150888414762));
#3213=CARTESIAN_POINT('Ctrl Pts',(0.00408869834201345,0.00291816670557086,
-0.000991626243178547));
#3214=CARTESIAN_POINT('Ctrl Pts',(0.00384728679499182,0.00333630379978535,
-0.00101680902829748));
#3215=CARTESIAN_POINT('Ctrl Pts',(0.00360651844477915,0.00375332681520823,
-0.00106216623675393));
#3216=CARTESIAN_POINT('Ctrl Pts',(0.00336575009456648,0.0041703498306311,
-0.00110752344521037));
#3217=CARTESIAN_POINT('Ctrl Pts',(0.0031256137510732,0.00458627817830528,
-0.00117308056854995));
#3218=CARTESIAN_POINT('Ctrl Pts',(0.00288675998197988,0.00499998504195424,
-0.00125470778672829));
#3219=CARTESIAN_POINT('',(0.00433012701892219,0.0025,0.003));
#3220=CARTESIAN_POINT('Ctrl Pts',(0.00288675134594208,0.00500000000001047,
0.00255341801261131));
#3221=CARTESIAN_POINT('Ctrl Pts',(0.00366025403784195,0.0036602540378486,
0.003));
#3222=CARTESIAN_POINT('Ctrl Pts',(0.00433012701892219,0.00250000000000001,
0.003));
#3223=CARTESIAN_POINT('Ctrl Pts',(0.00433012701892219,0.00250000000000001,
0.003));
#3224=CARTESIAN_POINT('Ctrl Pts',(0.00500000000000243,0.00133974596215141,
0.003));
#3225=CARTESIAN_POINT('Ctrl Pts',(0.0057735026919023,-1.04731475701905E-14,
0.00255341801261131));
#3226=CARTESIAN_POINT('Origin',(0.,-8.67361737988404E-19,0.003));
#3227=CARTESIAN_POINT('Origin',(0.,0.,0.003));
#3228=CARTESIAN_POINT('Origin',(0.,0.,0.003));
#3229=CARTESIAN_POINT('Origin',(0.,0.,0.003));
#3230=CARTESIAN_POINT('Origin',(0.,0.,0.003));
#3231=CARTESIAN_POINT('Origin',(0.,0.,0.003));
#3232=CARTESIAN_POINT('Origin',(0.,0.,0.003));
#3233=CARTESIAN_POINT('',(-0.003,-2.16854331959017E-19,0.003));
#3234=CARTESIAN_POINT('Origin',(0.,1.50539707785189E-19,0.003));
#3235=CARTESIAN_POINT('Origin',(0.,1.50539707785189E-19,0.003));
#3236=CARTESIAN_POINT('',(-0.0024585,-1.50539707785188E-19,0.0024585));
#3237=CARTESIAN_POINT('',(0.0024585,-1.50539707785188E-19,0.0024585));
#3238=CARTESIAN_POINT('Origin',(0.,1.50539707785189E-19,0.0024585));
#3239=CARTESIAN_POINT('',(0.0024585,1.50539707785189E-19,-0.0024585));
#3240=CARTESIAN_POINT('',(0.0024585,-1.50539707785188E-19,0.003));
#3241=CARTESIAN_POINT('Origin',(0.,1.50539707785189E-19,-0.0024585));
#3242=CARTESIAN_POINT('Origin',(0.,1.50539707785189E-19,0.0024585));
#3243=CARTESIAN_POINT('Origin',(0.,-8.67361737988404E-19,-0.003));
#3244=CARTESIAN_POINT('',(-0.00653289983773083,-8.00049487542732E-19,-0.003));
#3245=CARTESIAN_POINT('Origin',(0.,0.,-0.003));
#3246=CARTESIAN_POINT('',(0.003,1.50539707785189E-19,-0.003));
#3247=CARTESIAN_POINT('Origin',(0.,1.50539707785189E-19,-0.003));
#3248=CARTESIAN_POINT('Origin',(0.,0.,0.003));
#3249=CARTESIAN_POINT('Origin',(0.,0.,0.003));
#3250=CARTESIAN_POINT('Origin',(0.,0.,0.003));
#3251=CARTESIAN_POINT('Origin',(0.,0.,0.003));
#3252=CARTESIAN_POINT('Origin',(0.,0.,0.003));
#3253=CARTESIAN_POINT('Origin',(0.,0.,0.003));
#3254=CARTESIAN_POINT('Origin',(0.,0.,-0.0019));
#3255=CARTESIAN_POINT('',(-0.00672685951651014,-8.23802697520806E-19,-0.0019));
#3256=CARTESIAN_POINT('',(0.00672685951651014,-8.23802697520806E-19,-0.0019));
#3257=CARTESIAN_POINT('Origin',(0.,0.,-0.0019));
#3258=CARTESIAN_POINT('',(0.00609857484991769,3.11891280187063E-18,-0.00167132308271448));
#3259=CARTESIAN_POINT('',(0.00672685951651014,-8.23802697520806E-19,-0.0019));
#3260=CARTESIAN_POINT('',(0.00304928972140457,-0.00528151667910899,-0.0016713222184328));
#3261=CARTESIAN_POINT('Ctrl Pts',(0.00609857484991769,3.11891280187063E-18,
-0.00167132308271448));
#3262=CARTESIAN_POINT('Ctrl Pts',(0.00558687214450671,-0.000866849236070623,
-0.0014850785291514));
#3263=CARTESIAN_POINT('Ctrl Pts',(0.00455446054479797,-0.00262062618811301,
-0.00124956471272418));
#3264=CARTESIAN_POINT('Ctrl Pts',(0.00354470751944995,-0.00440396020586821,
-0.00148486875055949));
#3265=CARTESIAN_POINT('Ctrl Pts',(0.00304928972140457,-0.00528151667910899,
-0.0016713222184328));
#3266=CARTESIAN_POINT('',(-0.0030492825755407,-0.00528152070006659,-0.00167132218542784));
#3267=CARTESIAN_POINT('Ctrl Pts',(0.00304928742495884,-0.00528152074690959,
-0.00167132308271448));
#3268=CARTESIAN_POINT('Ctrl Pts',(0.00204272414259244,-0.00527179783765308,
-0.00148507881225216));
#3269=CARTESIAN_POINT('Ctrl Pts',(7.63893803576974E-6,-0.00525459158075091,
-0.00124956384220061));
#3270=CARTESIAN_POINT('Ctrl Pts',(-0.00204159528234752,-0.00527178693758448,
-0.00148487017016737));
#3271=CARTESIAN_POINT('Ctrl Pts',(-0.0030492825755407,-0.00528152070006659,
-0.00167132218542784));
#3272=CARTESIAN_POINT('',(-0.00609857240894841,-4.13512055109264E-9,-0.00167132219427486));
#3273=CARTESIAN_POINT('Ctrl Pts',(-0.00304928742495884,-0.00528152074690959,
-0.00167132308271448));
#3274=CARTESIAN_POINT('Ctrl Pts',(-0.00354414953194165,-0.00440494858680314,
-0.0014850785291514));
#3275=CARTESIAN_POINT('Ctrl Pts',(-0.00454675910347703,-0.00263396547651549,
-0.00124956471780991));
#3276=CARTESIAN_POINT('Ctrl Pts',(-0.00558629513036661,-0.000867826734172135,
-0.00148486874039706));
#3277=CARTESIAN_POINT('Ctrl Pts',(-0.00609857240894841,-4.13512055109264E-9,
-0.00167132219427486));
#3278=CARTESIAN_POINT('',(-0.00304928975931557,0.00528151661195546,-0.00167132220416477));
#3279=CARTESIAN_POINT('Ctrl Pts',(-0.00609857484991769,-1.32997605555308E-18,
-0.00167132308271448));
#3280=CARTESIAN_POINT('Ctrl Pts',(-0.00558687214450671,0.000866849236070624,
-0.0014850785291514));
#3281=CARTESIAN_POINT('Ctrl Pts',(-0.00455446055796522,0.00262062616574556,
-0.00124956471572788));
#3282=CARTESIAN_POINT('Ctrl Pts',(-0.00354470754520648,0.00440396016037937,
-0.0014848687445574));
#3283=CARTESIAN_POINT('Ctrl Pts',(-0.00304928975931557,0.00528151661195546,
-0.00167132220416477));
#3284=CARTESIAN_POINT('',(0.00304928284936602,0.00528152070271162,-0.00167132223609364));
#3285=CARTESIAN_POINT('Ctrl Pts',(-0.00304928742495884,0.00528152074690959,
-0.00167132308271448));
#3286=CARTESIAN_POINT('Ctrl Pts',(-0.00204272105198998,0.00527179780779938,
-0.0014850782403984));
#3287=CARTESIAN_POINT('Ctrl Pts',(-7.76376136486891E-6,0.00525459167257932,
-0.00124956559263654));
#3288=CARTESIAN_POINT('Ctrl Pts',(0.00204157993816983,0.0052717867891337,
-0.00148486731803956));
#3289=CARTESIAN_POINT('Ctrl Pts',(0.00304928284936602,0.00528152070271161,
-0.00167132223609364));
#3290=CARTESIAN_POINT('Ctrl Pts',(0.00304928742495884,0.00528152074690959,
-0.00167132308271448));
#3291=CARTESIAN_POINT('Ctrl Pts',(0.00354414953194165,0.00440494858680314,
-0.0014850785291514));
#3292=CARTESIAN_POINT('Ctrl Pts',(0.00454675915627546,0.00263396538325374,
-0.00124956470540752));
#3293=CARTESIAN_POINT('Ctrl Pts',(0.00558629523985264,0.000867826548158844,
-0.00148486876517975));
#3294=CARTESIAN_POINT('Ctrl Pts',(0.00609857257081076,3.86091785822701E-9,
-0.00167132225318787));
#3295=CARTESIAN_POINT('Origin',(0.,0.,-0.0019));
#3296=CARTESIAN_POINT('Origin',(0.,0.,-0.00243289983773083));
#3297=CARTESIAN_POINT('Origin',(-0.00653289983773083,-8.00049487542732E-19,
-0.00243289983773083));
#3298=CARTESIAN_POINT('Ctrl Pts',(-0.003392439652522,-0.005,-0.00134712277563101));
#3299=CARTESIAN_POINT('Ctrl Pts',(-0.00333573810031697,-0.00500000000000045,
-0.00163882427808492));
#3300=CARTESIAN_POINT('Ctrl Pts',(-0.00331969537168416,-0.00528446061132124,
-0.0017230905910049));
#3301=CARTESIAN_POINT('Ctrl Pts',(-0.00229932400794017,-0.005,-0.00113489737894972));
#3302=CARTESIAN_POINT('Ctrl Pts',(-0.0022699050095138,-0.00499999999999817,
-0.00142291384616243));
#3303=CARTESIAN_POINT('Ctrl Pts',(-0.00224289728430885,-0.00527390094042643,
-0.00151087013501245));
#3304=CARTESIAN_POINT('Ctrl Pts',(-3.29902936623155E-5,-0.005,-0.000850450941742578));
#3305=CARTESIAN_POINT('Ctrl Pts',(-3.26547606719844E-5,-0.00500000000000031,
-0.00112590779668));
#3306=CARTESIAN_POINT('Ctrl Pts',(-3.20185584867946E-5,-0.00525319396056387,
-0.00122643947342924));
#3307=CARTESIAN_POINT('Ctrl Pts',(0.00227701681215951,-0.005,-0.00112983249758146));
#3308=CARTESIAN_POINT('Ctrl Pts',(0.0022484543593711,-0.00500000000000123,
-0.0014177910180656));
#3309=CARTESIAN_POINT('Ctrl Pts',(0.0022208841466116,-0.00527363946899514,
-0.00150580534047564));
#3310=CARTESIAN_POINT('Ctrl Pts',(0.00339967250829873,-0.005,-0.00134857200053328));
#3311=CARTESIAN_POINT('Ctrl Pts',(0.00334288426086359,-0.00499999999999969,
-0.00164032138951496));
#3312=CARTESIAN_POINT('Ctrl Pts',(0.00332681896068871,-0.00528453549253266,
-0.00172453975783402));
#3313=CARTESIAN_POINT('Ctrl Pts',(-0.00288675134474064,-0.00500000000209144,
-0.00125471073847394));
#3314=CARTESIAN_POINT('Ctrl Pts',(-0.00288674885929026,-0.00500000430701771,
-0.00129742470408534));
#3315=CARTESIAN_POINT('Ctrl Pts',(-0.0028905782962394,-0.00500664507750752,
-0.00133965873446181));
#3316=CARTESIAN_POINT('Ctrl Pts',(-0.00290550747687201,-0.00503251662150569,
-0.00142447556160194));
#3317=CARTESIAN_POINT('Ctrl Pts',(-0.00291718276997192,-0.00505274378233935,
-0.00146593997083388));
#3318=CARTESIAN_POINT('Ctrl Pts',(-0.00294546681020174,-0.00510173821438759,
-0.00153843965802242));
#3319=CARTESIAN_POINT('Ctrl Pts',(-0.00296171097744791,-0.00512987415389936,
-0.00156974178652319));
#3320=CARTESIAN_POINT('Ctrl Pts',(-0.0029973641746807,-0.00519162567101304,
-0.00162283860847082));
#3321=CARTESIAN_POINT('Ctrl Pts',(-0.00301673813899042,-0.00522515254326503,
-0.00164476243573887));
#3322=CARTESIAN_POINT('Ctrl Pts',(-0.00304109722867609,-0.00526739574704128,
-0.00166516341250573));
#3323=CARTESIAN_POINT('Ctrl Pts',(-0.00304517979804077,-0.00527442761521776,
-0.00166834117515565));
#3324=CARTESIAN_POINT('Ctrl Pts',(-0.00304927734467971,-0.00528152350994555,
-0.00167132319559009));
#3325=CARTESIAN_POINT('Ctrl Pts',(0.00288675134836161,-0.005,-0.00125471114924454));
#3326=CARTESIAN_POINT('Ctrl Pts',(0.00288675631766473,-0.00500000000000004,
-0.0012974247085572));
#3327=CARTESIAN_POINT('Ctrl Pts',(0.00289059260464713,-0.00500663665536417,
-0.00133965834108164));
#3328=CARTESIAN_POINT('Ctrl Pts',(0.00290553325389396,-0.00503250117827399,
-0.00142447487127839));
#3329=CARTESIAN_POINT('Ctrl Pts',(0.00291721280449157,-0.00505272579460931,
-0.00146593933455075));
#3330=CARTESIAN_POINT('Ctrl Pts',(0.00294550149281011,-0.00510171820329803,
-0.00153843998343925));
#3331=CARTESIAN_POINT('Ctrl Pts',(0.00296174628749688,-0.00512985479605879,
-0.00156974282086848));
#3332=CARTESIAN_POINT('Ctrl Pts',(0.00299740088796859,-0.00519161200494954,
-0.00162284327160921));
#3333=CARTESIAN_POINT('Ctrl Pts',(0.00301675173212757,-0.00522515852632879,
-0.00164476913325231));
#3334=CARTESIAN_POINT('Ctrl Pts',(0.00304115183935638,-0.0052673686443409,
-0.0016651647029104));
#3335=CARTESIAN_POINT('Ctrl Pts',(0.0030452057973953,-0.00527442968077303,
-0.00166834749076532));
#3336=CARTESIAN_POINT('Ctrl Pts',(0.00304929520196274,-0.00528151399743187,
-0.00167132436916548));
#3337=CARTESIAN_POINT('Ctrl Pts',(0.00263483093370536,-0.00543633895346819,
-0.00134676459092806));
#3338=CARTESIAN_POINT('Ctrl Pts',(0.00266316771268226,-0.00538725821255638,
-0.00163845434397486));
#3339=CARTESIAN_POINT('Ctrl Pts',(0.00291752191368072,-0.00551558485545108,
-0.00172273174639874));
#3340=CARTESIAN_POINT('Ctrl Pts',(0.00318111242344103,-0.00449015165801158,
-0.00113472996117616));
#3341=CARTESIAN_POINT('Ctrl Pts',(0.00319582542346177,-0.0044646679944478,
-0.00142273422129603));
#3342=CARTESIAN_POINT('Ctrl Pts',(0.0034465028211626,-0.00457825537721831,
-0.00151070202086737));
#3343=CARTESIAN_POINT('Ctrl Pts',(0.00431379023378606,-0.00252829614188812,
-0.000850609795627995));
#3344=CARTESIAN_POINT('Ctrl Pts',(0.0043139544793176,-0.00252801166028083,
-0.00112606891836143));
#3345=CARTESIAN_POINT('Ctrl Pts',(0.004533552476125,-0.00265406372898638,
-0.00122659749600334));
#3346=CARTESIAN_POINT('Ctrl Pts',(0.00546798881062717,-0.000529165564775629,
-0.00112968126622273));
#3347=CARTESIAN_POINT('Ctrl Pts',(0.00545370297731455,-0.000553909353901215,
-0.00141762786335003));
#3348=CARTESIAN_POINT('Ctrl Pts',(0.00567690587397405,-0.000714562699553637,
-0.00150565341172077));
#3349=CARTESIAN_POINT('Ctrl Pts',(0.00602900688720259,0.000442546247817572,
-0.00134819896772613));
#3350=CARTESIAN_POINT('Ctrl Pts',(0.00600062712586943,0.000393391059281772,
-0.00163993606431589));
#3351=CARTESIAN_POINT('Ctrl Pts',(0.00623899133084267,0.00023722070282916,
-0.00172416606619949));
#3352=CARTESIAN_POINT('Ctrl Pts',(0.00577350269307922,2.04894862976534E-12,
-0.00125471073846544));
#3353=CARTESIAN_POINT('Ctrl Pts',(0.00577350515313831,4.26299629761274E-9,
-0.00129742442899938));
#3354=CARTESIAN_POINT('Ctrl Pts',(0.00578117082891029,8.21840813862419E-9,
-0.00133965819483664));
#3355=CARTESIAN_POINT('Ctrl Pts',(0.00581104059525994,1.48736200446331E-8,
-0.00142447497135105));
#3356=CARTESIAN_POINT('Ctrl Pts',(0.0058343954932902,1.73291284348548E-8,
-0.00146593954554163));
#3357=CARTESIAN_POINT('Ctrl Pts',(0.00589096860070516,1.98232300879166E-8,
-0.00153844019638302));
#3358=CARTESIAN_POINT('Ctrl Pts',(0.00592345795588389,1.99306575175446E-8,
-0.00156974296557482));
#3359=CARTESIAN_POINT('Ctrl Pts',(0.00599476839181334,1.91240807789401E-8,
-0.00162284326885734));
#3360=CARTESIAN_POINT('Ctrl Pts',(0.0060334956968563,4.3290744554038E-9,
-0.00164476902601384));
#3361=CARTESIAN_POINT('Ctrl Pts',(0.00608225115690581,3.0134882409869E-8,
-0.00166516477388993));
#3362=CARTESIAN_POINT('Ctrl Pts',(0.00609039298841603,1.06347343117895E-8,
-0.00166834748495594));
#3363=CARTESIAN_POINT('Ctrl Pts',(0.00609857319807417,1.00115177371027E-8,
-0.00167132447137854));
#3364=CARTESIAN_POINT('Ctrl Pts',(-0.00602542310434739,0.000436338953829055,
-0.00134676459100889));
#3365=CARTESIAN_POINT('Ctrl Pts',(-0.005997086325367,0.000387258212911715,
-0.00163845434406099));
#3366=CARTESIAN_POINT('Ctrl Pts',(-0.00623539755860201,0.000231144334731493,
-0.00172273174648082));
#3367=CARTESIAN_POINT('Ctrl Pts',(-0.00547914161454391,-0.000509848341744993,
-0.00113472996121131));
#3368=CARTESIAN_POINT('Ctrl Pts',(-0.00546442861452444,-0.000535332005308533,
-0.0014227342213371));
#3369=CARTESIAN_POINT('Ctrl Pts',(-0.00568813687240654,-0.00069563130849836,
-0.00151070202090343));
#3370=CARTESIAN_POINT('Ctrl Pts',(-0.00434646380406661,-0.00247170385809752,
-0.000850609795590723));
#3371=CARTESIAN_POINT('Ctrl Pts',(-0.00434629955853541,-0.00247198833970446,
-0.001126068918326));
#3372=CARTESIAN_POINT('Ctrl Pts',(-0.004565262850637,-0.00259913974920765,
-0.0012265974959679));
#3373=CARTESIAN_POINT('Ctrl Pts',(-0.00319226522706066,-0.00447083443549553,
-0.00112968126626212));
#3374=CARTESIAN_POINT('Ctrl Pts',(-0.00320655106037197,-0.00444609064636982,
-0.00141762786339413));
#3375=CARTESIAN_POINT('Ctrl Pts',(-0.00345728238725047,-0.00455906335224487,
-0.00150565341176094));
#3376=CARTESIAN_POINT('Ctrl Pts',(-0.00263124715043141,-0.00544254624818199,
-0.00134819896780807));
#3377=CARTESIAN_POINT('Ctrl Pts',(-0.00265962691176801,-0.00539339105964081,
-0.00163993606440357));
#3378=CARTESIAN_POINT('Ctrl Pts',(-0.00291405651026752,-0.00552173533827817,
-0.00172416606628272));
#3379=CARTESIAN_POINT('Ctrl Pts',(-0.00577350269307922,-2.04894842162822E-12,
-0.00125471073846544));
#3380=CARTESIAN_POINT('Ctrl Pts',(-0.00577350515315459,-4.26302450609168E-9,
-0.00129742471201551));
#3381=CARTESIAN_POINT('Ctrl Pts',(-0.00578117093028351,-8.21845998660043E-9,
-0.00133965875175794));
#3382=CARTESIAN_POINT('Ctrl Pts',(-0.00581104091458347,-1.48736587837042E-8,
-0.00142447558130857));
#3383=CARTESIAN_POINT('Ctrl Pts',(-0.00583439578648829,-1.7329148283752E-8,
-0.00146593997989766));
#3384=CARTESIAN_POINT('Ctrl Pts',(-0.00589096826521234,-1.98232085481949E-8,
-0.00153843971092982));
#3385=CARTESIAN_POINT('Ctrl Pts',(-0.00592345684890417,-1.99306575292987E-8,
-0.00156974187766182));
#3386=CARTESIAN_POINT('Ctrl Pts',(-0.00599476195176788,-1.91241658087579E-8,
-0.00162283873325911));
#3387=CARTESIAN_POINT('Ctrl Pts',(-0.00603348400147061,-4.35666052321621E-9,
-0.00164476252292788));
#3388=CARTESIAN_POINT('Ctrl Pts',(-0.00608224747444197,-3.0126263225575E-8,
-0.00166516355117631));
#3389=CARTESIAN_POINT('Ctrl Pts',(-0.0060903782558774,-1.06374662316222E-8,
-0.00166834120404817));
#3390=CARTESIAN_POINT('Ctrl Pts',(-0.00609857222254513,-1.0011591587375E-8,
-0.0016713232114511));
#3391=CARTESIAN_POINT('Ctrl Pts',(0.00602542310430558,-0.00043633895375665,
-0.00134676459099296));
#3392=CARTESIAN_POINT('Ctrl Pts',(0.00599708632532562,-0.000387258212840311,
-0.00163845434404502));
#3393=CARTESIAN_POINT('Ctrl Pts',(0.00623539755856036,-0.000231144334660519,
-0.00172273174646472));
#3394=CARTESIAN_POINT('Ctrl Pts',(0.00547914161451545,0.000509848341794287,
-0.00113472996120278));
#3395=CARTESIAN_POINT('Ctrl Pts',(0.00546442861449691,0.000535332005357402,
-0.00142273422132636));
#3396=CARTESIAN_POINT('Ctrl Pts',(0.00568813687237712,0.000695631308545852,
-0.00151070202089563));
#3397=CARTESIAN_POINT('Ctrl Pts',(0.0043464638040607,0.00247170385810776,
-0.000850609795600803));
#3398=CARTESIAN_POINT('Ctrl Pts',(0.00434629955852742,0.00247198833971471,
-0.00112606891833642));
#3399=CARTESIAN_POINT('Ctrl Pts',(0.00456526285063273,0.00259913974921762,
-0.00122659749597718));
#3400=CARTESIAN_POINT('Ctrl Pts',(0.00319226522710051,0.00447083443542652,
-0.00112968126625049));
#3401=CARTESIAN_POINT('Ctrl Pts',(0.00320655106041276,0.00444609064630528,
-0.0014176278633837));
#3402=CARTESIAN_POINT('Ctrl Pts',(0.00345728238728788,0.00455906335217811,
-0.00150565341175013));
#3403=CARTESIAN_POINT('Ctrl Pts',(0.00263124715047146,0.00544254624811262,
-0.00134819896779255));
#3404=CARTESIAN_POINT('Ctrl Pts',(0.00265962691180747,0.00539339105957097,
-0.00163993606438704));
#3405=CARTESIAN_POINT('Ctrl Pts',(0.00291405651030647,0.00552173533820915,
-0.00172416606626701));
#3406=CARTESIAN_POINT('Ctrl Pts',(0.00288675134479146,0.00500000000200342,
-0.00125471073845639));
#3407=CARTESIAN_POINT('Ctrl Pts',(0.00288674891221946,0.00500000421534183,
-0.00129742433834695));
#3408=CARTESIAN_POINT('Ctrl Pts',(0.00289057833514563,0.00500664479424417,
-0.00133965801827952));
#3409=CARTESIAN_POINT('Ctrl Pts',(0.00290550744416946,0.00503251593448348,
-0.00142447464062012));
#3410=CARTESIAN_POINT('Ctrl Pts',(0.00291718274092557,0.00505274299951618,
-0.00146593914613713));
#3411=CARTESIAN_POINT('Ctrl Pts',(0.0029454671218375,0.00510173791908386,
-0.00153843988171478));
#3412=CARTESIAN_POINT('Ctrl Pts',(0.00296171174464259,0.00512987464416147,
-0.00156974276006984));
#3413=CARTESIAN_POINT('Ctrl Pts',(0.00299736772729687,0.00519163102478694,
-0.00162284319962407));
#3414=CARTESIAN_POINT('Ctrl Pts',(0.00301674403056076,0.00522516248638102,
-0.00164476895368728));
#3415=CARTESIAN_POINT('Ctrl Pts',(0.00304109982315767,0.00526739903835552,
-0.0016651648357756));
#3416=CARTESIAN_POINT('Ctrl Pts',(0.0030451872163614,0.0052744400176427,
-0.00166834735963212));
#3417=CARTESIAN_POINT('Ctrl Pts',(0.00304927788497547,0.00528152402964165,
-0.00167132437123018));
#3418=CARTESIAN_POINT('Ctrl Pts',(-0.00263483093380463,0.00543633895329622,
-0.00134676459088959));
#3419=CARTESIAN_POINT('Ctrl Pts',(-0.00266316771278097,0.0053872582123861,
-0.00163845434394135));
#3420=CARTESIAN_POINT('Ctrl Pts',(-0.00291752191378344,0.00551558485528404,
-0.00172273174636237));
#3421=CARTESIAN_POINT('Ctrl Pts',(-0.00318111242350983,0.00449015165789242,
-0.00113472996115856));
#3422=CARTESIAN_POINT('Ctrl Pts',(-0.00319582542352974,0.00446466799432721,
-0.00142273422128192));
#3423=CARTESIAN_POINT('Ctrl Pts',(-0.00344650282123468,0.00457825537710422,
-0.00151070202085223));
#3424=CARTESIAN_POINT('Ctrl Pts',(-0.00431379023378665,0.00252829614188709,
-0.000850609795645256));
#3425=CARTESIAN_POINT('Ctrl Pts',(-0.00431395447931927,0.00252801166027967,
-0.00112606891838478));
#3426=CARTESIAN_POINT('Ctrl Pts',(-0.00453355247613352,0.00265406372898939,
-0.00122659749602347));
#3427=CARTESIAN_POINT('Ctrl Pts',(-0.00546798881055722,0.000529165564896799,
-0.00112968126620581));
#3428=CARTESIAN_POINT('Ctrl Pts',(-0.00545370297724336,0.000553909354023832,
-0.00141762786333782));
#3429=CARTESIAN_POINT('Ctrl Pts',(-0.0056769058739087,0.000714562699675378,
-0.00150565341170545));
#3430=CARTESIAN_POINT('Ctrl Pts',(-0.00602900688710061,-0.000442546247640928,
-0.0013481989676864));
#3431=CARTESIAN_POINT('Ctrl Pts',(-0.00600062712576853,-0.000393391059106834,
-0.0016399360642808));
#3432=CARTESIAN_POINT('Ctrl Pts',(-0.00623899133074701,-0.000237220702652166,
-0.00172416606616207));
#3433=CARTESIAN_POINT('Ctrl Pts',(-0.00288675134826077,0.005,-0.00125471027324244));
#3434=CARTESIAN_POINT('Ctrl Pts',(-0.00288675621269418,0.00499999999999996,
-0.00129742428190381));
#3435=CARTESIAN_POINT('Ctrl Pts',(-0.00289059247963899,0.00500663678669082,
-0.00133965836278528));
#3436=CARTESIAN_POINT('Ctrl Pts',(-0.00290553316002905,0.00503250164178277,
-0.00142447528722027));
#3437=CARTESIAN_POINT('Ctrl Pts',(-0.00291721269935843,0.00505272634054306,
-0.00146593974202318));
#3438=CARTESIAN_POINT('Ctrl Pts',(-0.00294550107180259,0.00510171830584963,
-0.00153843954266769));
#3439=CARTESIAN_POINT('Ctrl Pts',(-0.00296174544794714,0.00512985417813293,
-0.00156974173146961));
#3440=CARTESIAN_POINT('Ctrl Pts',(-0.00299739728854999,0.00519160657190795,
-0.00162283861855676));
#3441=CARTESIAN_POINT('Ctrl Pts',(-0.00301674558501153,0.00522514801552304,
-0.00164476237777865));
#3442=CARTESIAN_POINT('Ctrl Pts',(-0.00304114956668833,0.00526736597433145,
-0.00166516356742261));
#3443=CARTESIAN_POINT('Ctrl Pts',(-0.00304519818604292,0.00527441693996766,
-0.00166834116596992));
#3444=CARTESIAN_POINT('Ctrl Pts',(-0.00304929469773904,0.00528151354343759,
-0.00167132322067999));
#3445=CARTESIAN_POINT('Ctrl Pts',(0.00338841005797876,0.005,-0.00134634165980086));
#3446=CARTESIAN_POINT('Ctrl Pts',(0.00333176957023632,0.00500000000000039,
-0.00163801755763053));
#3447=CARTESIAN_POINT('Ctrl Pts',(0.00331572633073014,0.00528441681323915,
-0.0017223080413616));
#3448=CARTESIAN_POINT('Ctrl Pts',(0.0022964618679159,0.005,-0.00113452542043072));
#3449=CARTESIAN_POINT('Ctrl Pts',(0.00226702861060034,0.0049999999999983,
-0.00142251516960501));
#3450=CARTESIAN_POINT('Ctrl Pts',(0.00224010467644372,0.00527386950404515,
-0.00151049666360363));
#3451=CARTESIAN_POINT('Ctrl Pts',(3.22883156223924E-5,0.005,-0.000850800421083646));
#3452=CARTESIAN_POINT('Ctrl Pts',(3.19675726731644E-5,0.00500000000000161,
-0.00112626220337184));
#3453=CARTESIAN_POINT('Ctrl Pts',(3.13356900579081E-5,0.00525321490521392,
-0.00122678714678169));
#3454=CARTESIAN_POINT('Ctrl Pts',(-0.00227419770331868,0.005,-0.00112950336234551));
#3455=CARTESIAN_POINT('Ctrl Pts',(-0.00224561484281812,0.00499999999999842,
-0.00141743587027432));
#3456=CARTESIAN_POINT('Ctrl Pts',(-0.00221813611685098,0.00527361024641964,
-0.00150547469000147));
#3457=CARTESIAN_POINT('Ctrl Pts',(-0.00339548924405207,0.005,-0.00134775642748932));
#3458=CARTESIAN_POINT('Ctrl Pts',(-0.00333876378176818,0.00500000000000037,
-0.00163947896049063));
#3459=CARTESIAN_POINT('Ctrl Pts',(-0.0033226983415365,0.00528448991405657,
-0.00172372275338737));
#3460=CARTESIAN_POINT('Origin',(0.,1.50539707785189E-19,-0.003));
#3461=CARTESIAN_POINT('',(0.003,-2.16854331959017E-19,-0.003));
#3462=CARTESIAN_POINT('Origin',(0.,1.50539707785189E-19,0.0024585));
#3463=CARTESIAN_POINT('',(-0.0024585,-1.50539707785188E-19,0.0024585));
#3464=CARTESIAN_POINT('',(0.,0.,0.));
#3465=CARTESIAN_POINT('Origin',(0.03302,0.,-4.66590430475142E-19));
#3466=CARTESIAN_POINT('',(0.027604181732227,-0.00545787893630659,-0.00531751422345259));
#3467=CARTESIAN_POINT('',(0.0226758178125118,9.62593038363268E-18,0.00762));
#3468=CARTESIAN_POINT('Ctrl Pts',(0.027604181732227,-0.00545787893630659,
-0.00531751422345262));
#3469=CARTESIAN_POINT('Ctrl Pts',(0.0275279686032949,-0.00611737521333048,
-0.00464060943529688));
#3470=CARTESIAN_POINT('Ctrl Pts',(0.0274058826755258,-0.0066799041580939,
-0.00379613683788713));
#3471=CARTESIAN_POINT('Ctrl Pts',(0.0270288812884003,-0.00743795219517752,
-0.00194362990368062));
#3472=CARTESIAN_POINT('Ctrl Pts',(0.0267664171994647,-0.00762,-0.000931205111824686));
#3473=CARTESIAN_POINT('Ctrl Pts',(0.0261584464192118,-0.00762,0.000978832298277093));
#3474=CARTESIAN_POINT('Ctrl Pts',(0.0257672989424535,-0.00742146342376193,
0.00200253544380404));
#3475=CARTESIAN_POINT('Ctrl Pts',(0.0249302786493874,-0.00664164931271475,
0.00386998191769847));
#3476=CARTESIAN_POINT('Ctrl Pts',(0.0244863308943722,-0.00606132290844568,
0.00471498443683733));
#3477=CARTESIAN_POINT('Ctrl Pts',(0.0237267319642579,-0.0047360597713164,
0.00604024757396661));
#3478=CARTESIAN_POINT('Ctrl Pts',(0.023353947088258,-0.00390186974450739,
0.00662341729985035));
#3479=CARTESIAN_POINT('Ctrl Pts',(0.0228253280612608,-0.00203244645804173,
0.00741372953304487));
#3480=CARTESIAN_POINT('Ctrl Pts',(0.0226758178125118,-0.000995062388186708,
0.00762));
#3481=CARTESIAN_POINT('Ctrl Pts',(0.0226758178125118,1.66533453693773E-17,
0.00762));
#3482=CARTESIAN_POINT('',(0.027604181732227,0.00545787893630665,-0.00531751422345258));
#3483=CARTESIAN_POINT('Origin',(0.0270054795156059,0.,-4.66590430475142E-19));
#3484=CARTESIAN_POINT('Ctrl Pts',(0.0226758178125118,1.80411241501588E-17,
0.00762));
#3485=CARTESIAN_POINT('Ctrl Pts',(0.0226758178125118,0.000968408409381741,
0.00762));
#3486=CARTESIAN_POINT('Ctrl Pts',(0.0228174879353441,0.00198103471135963,
0.0074243825187784));
#3487=CARTESIAN_POINT('Ctrl Pts',(0.0233228057036299,0.00381368713962225,
0.00667096418394018));
#3488=CARTESIAN_POINT('Ctrl Pts',(0.0236805646112505,0.00463571714263501,
0.00611410121403885));
#3489=CARTESIAN_POINT('Ctrl Pts',(0.0244337098519972,0.00598793937687868,
0.00481301069798848));
#3490=CARTESIAN_POINT('Ctrl Pts',(0.0248888180929435,0.00659481223922085,
0.00395546133059954));
#3491=CARTESIAN_POINT('Ctrl Pts',(0.0257482260040042,0.0074113450160527,
0.00205163105595064));
#3492=CARTESIAN_POINT('Ctrl Pts',(0.0261504419883698,0.00762,0.00100397949753623));
#3493=CARTESIAN_POINT('Ctrl Pts',(0.0267667596758862,0.00762,-0.000932281056258697));
#3494=CARTESIAN_POINT('Ctrl Pts',(0.0270294385011349,0.00743753112566452,
-0.00194582582065931));
#3495=CARTESIAN_POINT('Ctrl Pts',(0.0274061392648596,0.00667871192581181,
-0.00379792191976084));
#3496=CARTESIAN_POINT('Ctrl Pts',(0.0275280372657644,0.00611678105529415,
-0.00464121927713181));
#3497=CARTESIAN_POINT('Ctrl Pts',(0.027604181732227,0.00545787893630661,
-0.00531751422345259));
#3498=CARTESIAN_POINT('',(0.0195416906937108,9.33180860950283E-19,0.00762));
#3499=CARTESIAN_POINT('',(0.03302,9.33180860950283E-19,0.00762));
#3500=CARTESIAN_POINT('',(0.0226351769200258,0.00396239491185587,-0.00650875));
#3501=CARTESIAN_POINT('Ctrl Pts',(0.0226351769200262,0.00396239491186084,
-0.00650874999999688));
#3502=CARTESIAN_POINT('Ctrl Pts',(0.0226703616592435,0.00449699874218484,
-0.00618329403731001));
#3503=CARTESIAN_POINT('Ctrl Pts',(0.0227049383031407,0.00498388799643907,
-0.00579469570810441));
#3504=CARTESIAN_POINT('Ctrl Pts',(0.022768434338136,0.00607818973523789,
-0.00469434328989012));
#3505=CARTESIAN_POINT('Ctrl Pts',(0.0227852939482288,0.00666267377651843,
-0.00383423955078307));
#3506=CARTESIAN_POINT('Ctrl Pts',(0.0226891534147118,0.00743351627485408,
-0.00195843047568892));
#3507=CARTESIAN_POINT('Ctrl Pts',(0.0225727993083733,0.00762,-0.000942950025364602));
#3508=CARTESIAN_POINT('Ctrl Pts',(0.022222087775008,0.00762,0.000991367009882884));
#3509=CARTESIAN_POINT('Ctrl Pts',(0.0219595192234926,0.00741593649953567,
0.00202962035276651));
#3510=CARTESIAN_POINT('Ctrl Pts',(0.0213461292163487,0.00661579385613863,
0.00391749182253754));
#3511=CARTESIAN_POINT('Ctrl Pts',(0.0209980046436713,0.00602056849457482,
0.00476834679472658));
#3512=CARTESIAN_POINT('Ctrl Pts',(0.0203927163583856,0.00467684447142528,
0.00608634155064048));
#3513=CARTESIAN_POINT('Ctrl Pts',(0.0200909975583043,0.00384158541585977,
0.00665672394664847));
#3514=CARTESIAN_POINT('Ctrl Pts',(0.0196624939401288,0.00198880319602538,
0.00742390702765397));
#3515=CARTESIAN_POINT('Ctrl Pts',(0.0195416906937108,0.000969608868230746,
0.00762));
#3516=CARTESIAN_POINT('Ctrl Pts',(0.0195416906937108,2.77555756156289E-19,
0.00762));
#3517=CARTESIAN_POINT('',(0.0226351769200258,-0.00396239491185566,-0.00650875));
#3518=CARTESIAN_POINT('Origin',(0.0233388317846976,0.,-4.66590430475142E-19));
#3519=CARTESIAN_POINT('Ctrl Pts',(0.0195416906937108,2.77555756156289E-19,
0.00762));
#3520=CARTESIAN_POINT('Ctrl Pts',(0.0195416906937108,-0.000969608868230745,
0.00762));
#3521=CARTESIAN_POINT('Ctrl Pts',(0.0196624939401288,-0.00198880319602538,
0.00742390702765397));
#3522=CARTESIAN_POINT('Ctrl Pts',(0.0200909975583043,-0.00384158541585977,
0.00665672394664847));
#3523=CARTESIAN_POINT('Ctrl Pts',(0.0203927163583856,-0.00467684447142528,
0.00608634155064048));
#3524=CARTESIAN_POINT('Ctrl Pts',(0.0209980046436713,-0.00602056849457482,
0.00476834679472658));
#3525=CARTESIAN_POINT('Ctrl Pts',(0.0213461292163487,-0.00661579385613863,
0.00391749182253753));
#3526=CARTESIAN_POINT('Ctrl Pts',(0.0219595192234926,-0.00741593649953567,
0.0020296203527665));
#3527=CARTESIAN_POINT('Ctrl Pts',(0.022222087775008,-0.00762000000000002,
0.000991367009882883));
#3528=CARTESIAN_POINT('Ctrl Pts',(0.0225727993083733,-0.00762000000000002,
-0.000942950025364605));
#3529=CARTESIAN_POINT('Ctrl Pts',(0.0226891534147118,-0.00743351627485408,
-0.00195843047568891));
#3530=CARTESIAN_POINT('Ctrl Pts',(0.0227852939482288,-0.00666267377651843,
-0.00383423955078307));
#3531=CARTESIAN_POINT('Ctrl Pts',(0.022768434338136,-0.00607818973523789,
-0.00469434328989012));
#3532=CARTESIAN_POINT('Ctrl Pts',(0.0227049383031407,-0.00498388799643903,
-0.00579469570810445));
#3533=CARTESIAN_POINT('Ctrl Pts',(0.0226703616592435,-0.00449699874218474,
-0.00618329403731008));
#3534=CARTESIAN_POINT('Ctrl Pts',(0.0226351769200262,-0.00396239491186069,
-0.00650874999999697));
#3535=CARTESIAN_POINT('Origin',(0.019796125,0.142748,0.0130716462696265));
#3536=CARTESIAN_POINT('',(0.019796125,0.0102506251722644,0.0110620425392529));
#3537=CARTESIAN_POINT('',(0.019796125,-0.0102506251722643,0.0110620425392529));
#3538=CARTESIAN_POINT('',(0.019796125,0.142748,0.0110620425392529));
#3539=CARTESIAN_POINT('Origin',(0.019796125,5.89805981832114E-17,2.47198095326695E-17));
#3540=CARTESIAN_POINT('Origin',(2.94902990916057E-17,0.142748,-0.0084254861247228));
#3541=CARTESIAN_POINT('',(0.0274949578025845,0.0217988744690902,-0.00446598692924329));
#3542=CARTESIAN_POINT('',(0.0217835558367569,0.012239066483666,0.0088118870380244));
#3543=CARTESIAN_POINT('Origin',(2.94902990916057E-17,0.0246496359780892,
-0.0084254861247228));
#3544=CARTESIAN_POINT('Ctrl Pts',(0.019796125,0.0102506251722644,0.0110620425392529));
#3545=CARTESIAN_POINT('Ctrl Pts',(0.0199250556804199,0.0103919650352694,
0.0109310701666171));
#3546=CARTESIAN_POINT('Ctrl Pts',(0.020053197009147,0.0105298129337859,
0.0107982953537534));
#3547=CARTESIAN_POINT('Ctrl Pts',(0.0201801831206385,0.0106640541437697,
0.0106640541437696));
#3548=CARTESIAN_POINT('Ctrl Pts',(0.0207051784182023,0.0112190440017391,
0.0101090642858003));
#3549=CARTESIAN_POINT('Ctrl Pts',(0.0212473394853561,0.0117511804678545,
0.00948952502387266));
#3550=CARTESIAN_POINT('Ctrl Pts',(0.0217835558367568,0.0122390664836661,
0.00881188703802442));
#3551=CARTESIAN_POINT('',(0.0272702604802117,-0.0147516885035667,-0.00313556818714528));
#3552=CARTESIAN_POINT('Ctrl Pts',(0.0272702604802117,-0.0147516885035667,
-0.00313556818714528));
#3553=CARTESIAN_POINT('Ctrl Pts',(0.0272495688109927,-0.0147743615770061,
-0.00302889976316783));
#3554=CARTESIAN_POINT('Ctrl Pts',(0.0272282288068284,-0.0147958237878268,
-0.00292223786676003));
#3555=CARTESIAN_POINT('Ctrl Pts',(0.027009028365588,-0.0149978474224452,
-0.0018591751296926));
#3556=CARTESIAN_POINT('Ctrl Pts',(0.0267588953224807,-0.0150812499999999,
-0.000907573932662182));
#3557=CARTESIAN_POINT('Ctrl Pts',(0.0261291401823591,-0.0150812499999999,
0.00107090252690661));
#3558=CARTESIAN_POINT('Ctrl Pts',(0.025713893024289,-0.0149657875440865,
0.00214629933068523));
#3559=CARTESIAN_POINT('Ctrl Pts',(0.0247544184553272,-0.0145148320065805,
0.00423096318224476));
#3560=CARTESIAN_POINT('Ctrl Pts',(0.0242102662610114,-0.0141796498547937,
0.00524033209572036));
#3561=CARTESIAN_POINT('Ctrl Pts',(0.0224519953219796,-0.0129007914315354,
0.008082788964929));
#3562=CARTESIAN_POINT('Ctrl Pts',(0.0211034211368484,-0.0116760800285812,
0.00972638603161029));
#3563=CARTESIAN_POINT('Ctrl Pts',(0.0198342735534848,-0.0102923878241089,
0.0110232329058798));
#3564=CARTESIAN_POINT('Ctrl Pts',(0.0198152109382652,-0.0102715480735547,
0.0110426543640688));
#3565=CARTESIAN_POINT('Ctrl Pts',(0.019796125,-0.0102506251722643,0.0110620425392529));
#3566=CARTESIAN_POINT('',(0.027604181732227,-0.0142879015563397,-0.00531751422345259));
#3567=CARTESIAN_POINT('Origin',(2.94902990916057E-17,-0.0136272817352386,
-0.0084254861247228));
#3568=CARTESIAN_POINT('',(0.027604181732227,0.142748,-0.00531751422345259));
#3569=CARTESIAN_POINT('',(0.027604181732227,0.0208616467784906,-0.00531751422345259));
#3570=CARTESIAN_POINT('',(0.027604181732227,0.142748,-0.00531751422345259));
#3571=CARTESIAN_POINT('Origin',(-0.0328868893532025,0.020918252442196,-0.0121903564161812));
#3572=CARTESIAN_POINT('Origin',(0.0303120908661135,0.142748,-0.0293684446117263));
#3573=CARTESIAN_POINT('',(0.0325400145420211,-0.00496968603632477,-0.0491562715255243));
#3574=CARTESIAN_POINT('',(0.0299860624391297,-0.00979121809375477,-0.0264727466343235));
#3575=CARTESIAN_POINT('',(0.0325400145420211,-0.009525,-0.0491562715255243));
#3576=CARTESIAN_POINT('',(0.0325400145420211,-0.00724734301816237,-0.0491562715255243));
#3577=CARTESIAN_POINT('',(0.03302,-0.009525,-0.053419375));
#3578=CARTESIAN_POINT('',(0.0327830114907868,-0.009525,-0.0513145059456507));
#3579=CARTESIAN_POINT('',(0.03302,0.0208616467784906,-0.053419375));
#3580=CARTESIAN_POINT('',(0.03302,0.022225,-0.053419375));
#3581=CARTESIAN_POINT('',(0.0303120908661135,0.0208616467784906,-0.0293684446117263));
#3582=CARTESIAN_POINT('Origin',(-0.017018,0.142748,0.0130716462696265));
#3583=CARTESIAN_POINT('',(-0.017018,0.0102506251722644,0.0110620425392529));
#3584=CARTESIAN_POINT('',(-0.017018,-0.0102506251722643,0.0110620425392529));
#3585=CARTESIAN_POINT('',(-0.017018,0.142748,0.0110620425392529));
#3586=CARTESIAN_POINT('Origin',(-0.017018,5.89805981832114E-17,2.47198095326695E-17));
#3587=CARTESIAN_POINT('Origin',(0.017018,0.142748,0.0130716462696265));
#3588=CARTESIAN_POINT('',(0.017018,-0.0102506251722643,0.0110620425392529));
#3589=CARTESIAN_POINT('',(0.017018,0.0102506251722644,0.0110620425392529));
#3590=CARTESIAN_POINT('Origin',(0.017018,5.89805981832114E-17,2.47198095326695E-17));
#3591=CARTESIAN_POINT('',(0.017018,0.142748,0.0110620425392529));
#3592=CARTESIAN_POINT('Origin',(-5.20417042793042E-18,0.142748,-0.0040616822293093));
#3593=CARTESIAN_POINT('',(0.0227482238351949,-0.0147516885035667,-0.00313556818714528));
#3594=CARTESIAN_POINT('',(0.0226351769200258,-0.0140346965755384,-0.00650875));
#3595=CARTESIAN_POINT('Origin',(-5.20417042793042E-18,-0.01455483688705,
-0.0040616822293093));
#3596=CARTESIAN_POINT('Ctrl Pts',(0.0227482238351949,-0.0147516885035667,
-0.00313556818714527));
#3597=CARTESIAN_POINT('Ctrl Pts',(0.0227446067595775,-0.0147705734226378,
-0.00304672162826799));
#3598=CARTESIAN_POINT('Ctrl Pts',(0.0227404659003224,-0.0147886314076116,
-0.00295781815060928));
#3599=CARTESIAN_POINT('Ctrl Pts',(0.0226851188015466,-0.0149930494779853,
-0.00190284970904404));
#3600=CARTESIAN_POINT('Ctrl Pts',(0.0225710627210582,-0.0150812499999999,
-0.000933372038593934));
#3601=CARTESIAN_POINT('Ctrl Pts',(0.0222119151141167,-0.0150812499999999,
0.00104747338045759));
#3602=CARTESIAN_POINT('Ctrl Pts',(0.0219431733917285,-0.0149706590076676,
0.00210320147053684));
#3603=CARTESIAN_POINT('Ctrl Pts',(0.0212601083230291,-0.0145354311779761,
0.00415515679714474));
#3604=CARTESIAN_POINT('Ctrl Pts',(0.0208459021049179,-0.0142110577693777,
0.00515147888694799));
#3605=CARTESIAN_POINT('Ctrl Pts',(0.0194466634913425,-0.0129714177672581,
0.00796100440593939));
#3606=CARTESIAN_POINT('Ctrl Pts',(0.0182957954663637,-0.0117801714359752,
0.0095915927647639));
#3607=CARTESIAN_POINT('Ctrl Pts',(0.0171380411001156,-0.0103958203260114,
0.0109261520357052));
#3608=CARTESIAN_POINT('Ctrl Pts',(0.0170781669004994,-0.0103236873082037,
0.0109943396202718));
#3609=CARTESIAN_POINT('Ctrl Pts',(0.017018,-0.0102506251722643,0.0110620425392529));
#3610=CARTESIAN_POINT('',(0.0187779282455329,0.012239066483666,0.0088118870380244));
#3611=CARTESIAN_POINT('Ctrl Pts',(0.017018,0.0102506251722644,0.0110620425392529));
#3612=CARTESIAN_POINT('Ctrl Pts',(0.0170781669004994,0.0103236873082038,
0.0109943396202718));
#3613=CARTESIAN_POINT('Ctrl Pts',(0.0171380411001156,0.0103958203260115,
0.0109261520357052));
#3614=CARTESIAN_POINT('Ctrl Pts',(0.017721633324578,0.011093633754536,0.0102534373076843));
#3615=CARTESIAN_POINT('Ctrl Pts',(0.018259156437714,0.0116942557001332,
0.00956858936204477));
#3616=CARTESIAN_POINT('Ctrl Pts',(0.0187779282455329,0.0122390664836661,
0.00881188703802446));
#3617=CARTESIAN_POINT('',(0.0226351769200258,0.0232696236842349,-0.00650875));
#3618=CARTESIAN_POINT('Origin',(-5.20417042793042E-18,0.0215077830407108,
-0.0040616822293093));
#3619=CARTESIAN_POINT('',(0.0226351769200258,0.142748,-0.00650875));
#3620=CARTESIAN_POINT('',(0.0226351769200258,0.142748,-0.00650875));
#3621=CARTESIAN_POINT('Origin',(2.42861286636753E-17,0.142748,-0.00406168222930931));
#3622=CARTESIAN_POINT('',(-0.0226351769200258,-0.0140346965755384,-0.00650875));
#3623=CARTESIAN_POINT('',(-0.0227482238351949,-0.0147516885035667,-0.00313556818714528));
#3624=CARTESIAN_POINT('Origin',(2.42861286636753E-17,-0.01455483688705,
-0.00406168222930931));
#3625=CARTESIAN_POINT('',(-0.0226351769200258,-0.00396239491185574,-0.00650875));
#3626=CARTESIAN_POINT('',(-0.0226351769200258,0.142748,-0.00650875));
#3627=CARTESIAN_POINT('',(-0.0195416906937107,9.33180860950283E-19,0.00762));
#3628=CARTESIAN_POINT('Ctrl Pts',(-0.0226351769200261,-0.00396239491186075,
-0.00650874999999693));
#3629=CARTESIAN_POINT('Ctrl Pts',(-0.0226703616592435,-0.00449699874218478,
-0.00618329403731005));
#3630=CARTESIAN_POINT('Ctrl Pts',(-0.0227049383031407,-0.00498388799643905,
-0.00579469570810443));
#3631=CARTESIAN_POINT('Ctrl Pts',(-0.022768434338136,-0.00607818973523789,
-0.00469434328989012));
#3632=CARTESIAN_POINT('Ctrl Pts',(-0.0227852939482288,-0.00666267377651843,
-0.00383423955078307));
#3633=CARTESIAN_POINT('Ctrl Pts',(-0.0226891534147118,-0.00743351627485408,
-0.00195843047568891));
#3634=CARTESIAN_POINT('Ctrl Pts',(-0.0225727993083733,-0.00762000000000002,
-0.000942950025364604));
#3635=CARTESIAN_POINT('Ctrl Pts',(-0.0222220877750079,-0.00762000000000002,
0.000991367009882883));
#3636=CARTESIAN_POINT('Ctrl Pts',(-0.0219595192234926,-0.00741593649953567,
0.0020296203527665));
#3637=CARTESIAN_POINT('Ctrl Pts',(-0.0213461292163486,-0.00661579385613864,
0.00391749182253753));
#3638=CARTESIAN_POINT('Ctrl Pts',(-0.0209980046436713,-0.00602056849457482,
0.00476834679472658));
#3639=CARTESIAN_POINT('Ctrl Pts',(-0.0203927163583856,-0.00467684447142528,
0.00608634155064047));
#3640=CARTESIAN_POINT('Ctrl Pts',(-0.0200909975583043,-0.00384158541585977,
0.00665672394664846));
#3641=CARTESIAN_POINT('Ctrl Pts',(-0.0196624939401288,-0.00198880319602538,
0.00742390702765397));
#3642=CARTESIAN_POINT('Ctrl Pts',(-0.0195416906937107,-0.000969608868230746,
0.00762));
#3643=CARTESIAN_POINT('Ctrl Pts',(-0.0195416906937107,-2.77555756156289E-19,
0.00762));
#3644=CARTESIAN_POINT('',(-0.0226351769200258,0.0039623949118558,-0.00650875));
#3645=CARTESIAN_POINT('Ctrl Pts',(-0.0195416906937107,0.,0.00762));
#3646=CARTESIAN_POINT('Ctrl Pts',(-0.0195416906937107,0.000969608868230746,
0.00762));
#3647=CARTESIAN_POINT('Ctrl Pts',(-0.0196624939401288,0.00198880319602538,
0.00742390702765397));
#3648=CARTESIAN_POINT('Ctrl Pts',(-0.0200909975583043,0.00384158541585977,
0.00665672394664847));
#3649=CARTESIAN_POINT('Ctrl Pts',(-0.0203927163583856,0.00467684447142528,
0.00608634155064048));
#3650=CARTESIAN_POINT('Ctrl Pts',(-0.0209980046436713,0.00602056849457482,
0.00476834679472658));
#3651=CARTESIAN_POINT('Ctrl Pts',(-0.0213461292163486,0.00661579385613863,
0.00391749182253754));
#3652=CARTESIAN_POINT('Ctrl Pts',(-0.0219595192234926,0.00741593649953567,
0.00202962035276651));
#3653=CARTESIAN_POINT('Ctrl Pts',(-0.0222220877750079,0.00762,0.000991367009882883));
#3654=CARTESIAN_POINT('Ctrl Pts',(-0.0225727993083733,0.00762,-0.000942950025364602));
#3655=CARTESIAN_POINT('Ctrl Pts',(-0.0226891534147118,0.00743351627485408,
-0.00195843047568892));
#3656=CARTESIAN_POINT('Ctrl Pts',(-0.0227852939482288,0.00666267377651843,
-0.00383423955078308));
#3657=CARTESIAN_POINT('Ctrl Pts',(-0.022768434338136,0.00607818973523789,
-0.00469434328989012));
#3658=CARTESIAN_POINT('Ctrl Pts',(-0.0227049383031407,0.00498388799643906,
-0.00579469570810442));
#3659=CARTESIAN_POINT('Ctrl Pts',(-0.0226703616592435,0.00449699874218481,
-0.00618329403731003));
#3660=CARTESIAN_POINT('Ctrl Pts',(-0.0226351769200261,0.00396239491186079,
-0.00650874999999691));
#3661=CARTESIAN_POINT('',(-0.0226351769200258,0.0232696236842349,-0.00650875));
#3662=CARTESIAN_POINT('',(-0.0226351769200258,0.142748,-0.00650875));
#3663=CARTESIAN_POINT('',(-0.0187779282455329,0.012239066483666,0.0088118870380244));
#3664=CARTESIAN_POINT('Origin',(2.42861286636753E-17,0.0215077830407108,
-0.00406168222930931));
#3665=CARTESIAN_POINT('Ctrl Pts',(-0.0187779282455329,0.0122390664836661,
0.00881188703802446));
#3666=CARTESIAN_POINT('Ctrl Pts',(-0.0183124690330524,0.0117502442415317,
0.00949082537374769));
#3667=CARTESIAN_POINT('Ctrl Pts',(-0.017832992880629,0.0112176146967558,
0.0101104935907835));
#3668=CARTESIAN_POINT('Ctrl Pts',(-0.0172495397298473,0.0105296488003802,
0.0107984594871591));
#3669=CARTESIAN_POINT('Ctrl Pts',(-0.0171342563174104,0.0103917980562914,
0.0109312248974374));
#3670=CARTESIAN_POINT('Ctrl Pts',(-0.017018,0.0102506251722644,0.0110620425392529));
#3671=CARTESIAN_POINT('Ctrl Pts',(-0.017018,-0.0102506251722643,0.0110620425392529));
#3672=CARTESIAN_POINT('Ctrl Pts',(-0.0170781669004994,-0.0103236873082037,
0.0109943396202718));
#3673=CARTESIAN_POINT('Ctrl Pts',(-0.0171380411001156,-0.0103958203260114,
0.0109261520357052));
#3674=CARTESIAN_POINT('Ctrl Pts',(-0.0182957954663637,-0.0117801714359752,
0.00959159276476389));
#3675=CARTESIAN_POINT('Ctrl Pts',(-0.0194466634913425,-0.0129714177672581,
0.00796100440593937));
#3676=CARTESIAN_POINT('Ctrl Pts',(-0.0208459021049179,-0.0142110577693777,
0.00515147888694798));
#3677=CARTESIAN_POINT('Ctrl Pts',(-0.0212601083230291,-0.0145354311779761,
0.00415515679714473));
#3678=CARTESIAN_POINT('Ctrl Pts',(-0.0219431733917285,-0.0149706590076676,
0.00210320147053683));
#3679=CARTESIAN_POINT('Ctrl Pts',(-0.0222119151141167,-0.0150812499999999,
0.00104747338045759));
#3680=CARTESIAN_POINT('Ctrl Pts',(-0.0225710627210582,-0.0150812499999999,
-0.000933372038593937));
#3681=CARTESIAN_POINT('Ctrl Pts',(-0.0226851188015466,-0.0149930494779853,
-0.00190284970904404));
#3682=CARTESIAN_POINT('Ctrl Pts',(-0.0227404659003224,-0.0147886314076116,
-0.00295781815060928));
#3683=CARTESIAN_POINT('Ctrl Pts',(-0.0227446067595775,-0.0147705734226378,
-0.003046721628268));
#3684=CARTESIAN_POINT('Ctrl Pts',(-0.0227482238351949,-0.0147516885035667,
-0.00313556818714527));
#3685=CARTESIAN_POINT('Origin',(0.0214187310324227,0.142748,-0.0177607750600836));
#3686=CARTESIAN_POINT('',(0.0202022851448196,0.0394720969546926,-0.0290128001201673));
#3687=CARTESIAN_POINT('',(0.0202022851448196,-0.00925131305834584,-0.0290128001201673));
#3688=CARTESIAN_POINT('',(0.0202022851448196,0.142748,-0.0290128001201673));
#3689=CARTESIAN_POINT('',(0.0206505404826075,-0.0101326416961916,-0.0248664748742124));
#3690=CARTESIAN_POINT('',(0.0212486442437504,0.0325035973672875,-0.019334063956889));
#3691=CARTESIAN_POINT('Origin',(-2.20309881449055E-16,0.142748,-0.02682875));
#3692=CARTESIAN_POINT('',(-0.0202022851448196,-0.00925131305834583,-0.0290128001201673));
#3693=CARTESIAN_POINT('Origin',(-2.20309881449055E-16,-0.00971554724240362,
-0.02682875));
#3694=CARTESIAN_POINT('',(-0.0202022851448196,0.0394720969546926,-0.0290128001201673));
#3695=CARTESIAN_POINT('Origin',(-2.20309881449055E-16,0.0378996238441018,
-0.02682875));
#3696=CARTESIAN_POINT('',(-0.0202022851448196,0.142748,-0.0290128001201673));
#3697=CARTESIAN_POINT('Origin',(-0.0214187310324227,0.142748,-0.0177607750600836));
#3698=CARTESIAN_POINT('',(-0.0199202248773828,-0.00869674567155872,-0.0316218345457809));
#3699=CARTESIAN_POINT('',(-0.020744188550585,0.0358631507875988,-0.0240002378977473));
#3700=CARTESIAN_POINT('Origin',(-0.0233388317846976,0.,-4.66590430475142E-19));
#3701=CARTESIAN_POINT('Origin',(0.03302,-0.009525,-0.0512878232627621));
#3702=CARTESIAN_POINT('',(-0.032540014542021,-0.009525,-0.0491562715255243));
#3703=CARTESIAN_POINT('',(0.03302,-0.009525,-0.0491562715255243));
#3704=CARTESIAN_POINT('',(-0.03302,-0.009525,-0.053419375));
#3705=CARTESIAN_POINT('',(-0.0319563253038297,-0.009525,-0.0439720985928172));
#3706=CARTESIAN_POINT('',(0.03302,-0.009525,-0.053419375));
#3707=CARTESIAN_POINT('Origin',(0.03302,-0.00724734301816237,-0.0491562715255243));
#3708=CARTESIAN_POINT('',(-0.0325400145420211,-0.00496968603632477,-0.0491562715255243));
#3709=CARTESIAN_POINT('',(0.03302,-0.00496968603632477,-0.0491562715255243));
#3710=CARTESIAN_POINT('',(-0.032540014542021,-0.00724734301816237,-0.0491562715255243));
#3711=CARTESIAN_POINT('Origin',(0.03302,-0.00986068726994574,-0.0261459198563348));
#3712=CARTESIAN_POINT('',(-0.0272702604802117,-0.0147516885035667,-0.00313556818714528));
#3713=CARTESIAN_POINT('',(0.03302,-0.0147516885035667,-0.0031355681871453));
#3714=CARTESIAN_POINT('',(-0.027604181732227,-0.0142879015563397,-0.00531751422345259));
#3715=CARTESIAN_POINT('Origin',(2.25514051876985E-17,-0.0136272817352386,
-0.0084254861247228));
#3716=CARTESIAN_POINT('',(-0.0291946834112552,-0.0112852395940622,-0.0194439280997692));
#3717=CARTESIAN_POINT('',(0.03302,-0.0147516885035667,-0.0031355681871453));
#3718=CARTESIAN_POINT('Origin',(0.03302,5.89805981832114E-17,2.47198095326695E-17));
#3719=CARTESIAN_POINT('',(0.03302,0.012239066483666,0.0088118870380244));
#3720=CARTESIAN_POINT('Origin',(0.03302,5.89805981832114E-17,2.47198095326695E-17));
#3721=CARTESIAN_POINT('',(-0.0217835558367568,0.012239066483666,0.0088118870380244));
#3722=CARTESIAN_POINT('',(0.03302,0.012239066483666,0.0088118870380244));
#3723=CARTESIAN_POINT('',(-0.019796125,0.0102506251722644,0.0110620425392529));
#3724=CARTESIAN_POINT('Ctrl Pts',(-0.0217835558367568,0.0122390664836661,
0.00881188703802445));
#3725=CARTESIAN_POINT('Ctrl Pts',(-0.0212473394853562,0.0117511804678545,
0.00948952502387266));
#3726=CARTESIAN_POINT('Ctrl Pts',(-0.0207051784182024,0.0112190440017391,
0.0101090642858003));
#3727=CARTESIAN_POINT('Ctrl Pts',(-0.0201801831206385,0.0106640541437697,
0.0106640541437697));
#3728=CARTESIAN_POINT('Ctrl Pts',(-0.020053197009147,0.0105298129337859,
0.0107982953537535));
#3729=CARTESIAN_POINT('Ctrl Pts',(-0.01992505568042,0.0103919650352694,
0.0109310701666172));
#3730=CARTESIAN_POINT('Ctrl Pts',(-0.019796125,0.0102506251722644,0.0110620425392529));
#3731=CARTESIAN_POINT('',(-0.019796125,-0.0102506251722643,0.0110620425392529));
#3732=CARTESIAN_POINT('Origin',(-0.019796125,5.89805981832114E-17,2.47198095326695E-17));
#3733=CARTESIAN_POINT('Ctrl Pts',(-0.019796125,-0.0102506251722643,0.0110620425392529));
#3734=CARTESIAN_POINT('Ctrl Pts',(-0.0198152109382653,-0.0102715480735547,
0.0110426543640688));
#3735=CARTESIAN_POINT('Ctrl Pts',(-0.0198342735534848,-0.0102923878241089,
0.0110232329058798));
#3736=CARTESIAN_POINT('Ctrl Pts',(-0.0211034211368485,-0.0116760800285813,
0.00972638603161028));
#3737=CARTESIAN_POINT('Ctrl Pts',(-0.0224519953219796,-0.0129007914315354,
0.00808278896492899));
#3738=CARTESIAN_POINT('Ctrl Pts',(-0.0242102662610114,-0.0141796498547937,
0.00524033209572035));
#3739=CARTESIAN_POINT('Ctrl Pts',(-0.0247544184553273,-0.0145148320065805,
0.00423096318224475));
#3740=CARTESIAN_POINT('Ctrl Pts',(-0.025713893024289,-0.0149657875440865,
0.00214629933068522));
#3741=CARTESIAN_POINT('Ctrl Pts',(-0.0261291401823591,-0.0150812499999999,
0.0010709025269066));
#3742=CARTESIAN_POINT('Ctrl Pts',(-0.0267588953224807,-0.0150812499999999,
-0.000907573932662187));
#3743=CARTESIAN_POINT('Ctrl Pts',(-0.027009028365588,-0.0149978474224452,
-0.0018591751296926));
#3744=CARTESIAN_POINT('Ctrl Pts',(-0.0272282288068284,-0.0147958237878268,
-0.00292223786676003));
#3745=CARTESIAN_POINT('Ctrl Pts',(-0.0272495688109927,-0.0147743615770061,
-0.00302889976316783));
#3746=CARTESIAN_POINT('Ctrl Pts',(-0.0272702604802117,-0.0147516885035667,
-0.00313556818714527));
#3747=CARTESIAN_POINT('Origin',(0.03302,0.033107033241833,-0.0201721922437499));
#3748=CARTESIAN_POINT('',(-0.0274949578025847,0.0217988744690917,-0.00446598692924536));
#3749=CARTESIAN_POINT('',(1.03779831950312E-15,0.0539658339565387,-0.0491435405616761));
#3750=CARTESIAN_POINT('Origin',(0.00596083144644427,0.0208616467784906,
-0.00316424622761118));
#3751=CARTESIAN_POINT('Origin',(2.25514051876985E-17,0.0246496359780892,
-0.0084254861247228));
#3752=CARTESIAN_POINT('Origin',(-0.00596083144644428,0.0208616467784906,
-0.00316424622761117));
#3753=CARTESIAN_POINT('Origin',(0.03302,0.022225,-0.053419375));
#3754=CARTESIAN_POINT('',(-0.03302,0.0208616467784906,-0.053419375));
#3755=CARTESIAN_POINT('',(-0.03302,0.022225,-0.053419375));
#3756=CARTESIAN_POINT('',(1.4662354446901E-13,0.0539736348755679,-0.053419375));
#3757=CARTESIAN_POINT('Origin',(0.000302575402688698,0.0208616467784906,
-0.053419375));
#3758=CARTESIAN_POINT('Origin',(-0.000302575402688701,0.0208616467784906,
-0.053419375));
#3759=CARTESIAN_POINT('Origin',(0.03302,0.,-4.66590430475142E-19));
#3760=CARTESIAN_POINT('',(-0.0226758178125118,1.89034674318853E-19,0.00762));
#3761=CARTESIAN_POINT('',(0.03302,9.33180860950283E-19,0.00762));
#3762=CARTESIAN_POINT('',(-0.027604181732227,0.00545787893630664,-0.00531751422345259));
#3763=CARTESIAN_POINT('Ctrl Pts',(-0.027604181732227,0.00545787893630661,
-0.0053175142234526));
#3764=CARTESIAN_POINT('Ctrl Pts',(-0.0275280372657645,0.00611678105529414,
-0.00464121927713182));
#3765=CARTESIAN_POINT('Ctrl Pts',(-0.0274061392648596,0.00667871192581181,
-0.00379792191976086));
#3766=CARTESIAN_POINT('Ctrl Pts',(-0.0270294385011349,0.00743753112566452,
-0.00194582582065932));
#3767=CARTESIAN_POINT('Ctrl Pts',(-0.0267667596758862,0.00761999999999999,
-0.000932281056258699));
#3768=CARTESIAN_POINT('Ctrl Pts',(-0.0261504419883699,0.00761999999999999,
0.00100397949753623));
#3769=CARTESIAN_POINT('Ctrl Pts',(-0.0257482260040043,0.0074113450160527,
0.00205163105595065));
#3770=CARTESIAN_POINT('Ctrl Pts',(-0.0248888180929436,0.00659481223922084,
0.00395546133059956));
#3771=CARTESIAN_POINT('Ctrl Pts',(-0.0244337098519972,0.00598793937687863,
0.00481301069798849));
#3772=CARTESIAN_POINT('Ctrl Pts',(-0.0236805646112506,0.00463571714263495,
0.00611410121403885));
#3773=CARTESIAN_POINT('Ctrl Pts',(-0.02332280570363,0.00381368713962221,
0.0066709641839402));
#3774=CARTESIAN_POINT('Ctrl Pts',(-0.0228174879353442,0.0019810347113596,
0.00742438251877841));
#3775=CARTESIAN_POINT('Ctrl Pts',(-0.0226758178125118,0.000968408409381716,
0.00762));
#3776=CARTESIAN_POINT('Ctrl Pts',(-0.0226758178125118,8.32667268468867E-19,
0.00762));
#3777=CARTESIAN_POINT('',(-0.027604181732227,-0.00545787893630657,-0.00531751422345261));
#3778=CARTESIAN_POINT('Origin',(-0.0270054795156059,0.,-4.66590430475142E-19));
#3779=CARTESIAN_POINT('Ctrl Pts',(-0.0226758178125118,-5.55111512312578E-19,
0.00762));
#3780=CARTESIAN_POINT('Ctrl Pts',(-0.0226758178125118,-0.000968408409381723,
0.00762));
#3781=CARTESIAN_POINT('Ctrl Pts',(-0.0228174879353442,-0.00198103471135961,
0.00742438251877841));
#3782=CARTESIAN_POINT('Ctrl Pts',(-0.02332280570363,-0.00381368713962224,
0.00667096418394019));
#3783=CARTESIAN_POINT('Ctrl Pts',(-0.0236805646112506,-0.00463571714263499,
0.00611410121403885));
#3784=CARTESIAN_POINT('Ctrl Pts',(-0.0244337098519972,-0.00598793937687866,
0.00481301069798848));
#3785=CARTESIAN_POINT('Ctrl Pts',(-0.0248888180929436,-0.00659481223922085,
0.00395546133059954));
#3786=CARTESIAN_POINT('Ctrl Pts',(-0.0257482260040043,-0.0074113450160527,
0.00205163105595064));
#3787=CARTESIAN_POINT('Ctrl Pts',(-0.0261504419883699,-0.00762000000000002,
0.00100397949753623));
#3788=CARTESIAN_POINT('Ctrl Pts',(-0.0267667596758862,-0.00762000000000002,
-0.000932281056258699));
#3789=CARTESIAN_POINT('Ctrl Pts',(-0.0270294385011349,-0.00743753112566452,
-0.00194582582065931));
#3790=CARTESIAN_POINT('Ctrl Pts',(-0.0274061392648597,-0.0066787119258118,
-0.00379792191976087));
#3791=CARTESIAN_POINT('Ctrl Pts',(-0.0275280372657645,-0.00611678105529412,
-0.00464121927713185));
#3792=CARTESIAN_POINT('Ctrl Pts',(-0.027604181732227,-0.00545787893630657,
-0.00531751422345264));
#3793=CARTESIAN_POINT('Origin',(-0.019796125,0.142748,0.0130716462696265));
#3794=CARTESIAN_POINT('',(-0.019796125,0.142748,0.0110620425392529));
#3795=CARTESIAN_POINT('Origin',(2.25514051876985E-17,0.142748,-0.0084254861247228));
#3796=CARTESIAN_POINT('',(-0.027604181732227,0.0208616467784906,-0.00531751422345259));
#3797=CARTESIAN_POINT('',(-0.027604181732227,0.142748,-0.00531751422345259));
#3798=CARTESIAN_POINT('',(-0.027604181732227,0.142748,-0.00531751422345259));
#3799=CARTESIAN_POINT('Origin',(0.0328868894519471,0.0209182515429762,-0.012190355439119));
#3800=CARTESIAN_POINT('Origin',(-0.0303120908661135,0.142748,-0.0293684446117263));
#3801=CARTESIAN_POINT('',(-0.0303120908661135,0.0208616467784906,-0.0293684446117263));
#3802=CARTESIAN_POINT('Origin',(0.000949119378095248,0.0208616467784906,
-0.047676942969741));
#3803=CARTESIAN_POINT('Origin',(-2.00577401909819E-18,0.0208616467784906,
-0.0561067694388323));
#3804=CARTESIAN_POINT('Origin',(-0.000122433191138131,0.0208616467784906,
-0.0550193503225745));
#3805=CARTESIAN_POINT('',(0.,0.,0.));
#3806=CARTESIAN_POINT('',(0.,0.,0.));
#3807=CARTESIAN_POINT('',(-0.448100716117138,-0.834500123492625,-0.0844193750000001));
#3808=CARTESIAN_POINT('',(-0.0331007161171427,0.0504998765073697,-0.059419375));
#3809=CARTESIAN_POINT('',(-0.0331007161171427,0.0504998765073697,-0.050419375));
#3810=CARTESIAN_POINT('',(0.0368992838828569,0.0504998765073698,-0.059419375));
#3811=CARTESIAN_POINT('',(0.0368992838828569,-0.0195001234926293,-0.0594193750000001));
#3812=CARTESIAN_POINT('',(-0.0314152123959047,-0.0195001234926298,-0.059419375));
#3813=CARTESIAN_POINT('',(-0.0314152123959047,-0.0195001234926298,-0.050419375));
#3814=CARTESIAN_POINT('',(0.0368992838828569,0.0504998765073698,-0.050419375));
#3815=CARTESIAN_POINT('',(0.0368992838828569,-0.0195001234926293,-0.050419375));
#3816=CARTESIAN_POINT('',(0.,0.,0.));
#3817=UNCERTAINTY_MEASURE_WITH_UNIT(LENGTH_MEASURE(1.E-5),#3833,
'DISTANCE_ACCURACY_VALUE',
'Maximum model space distance between geometric entities at asserted c
onnectivities');
#3818=UNCERTAINTY_MEASURE_WITH_UNIT(LENGTH_MEASURE(1.E-5),#3833,
'DISTANCE_ACCURACY_VALUE',
'Maximum model space distance between geometric entities at asserted c
onnectivities');
#3819=UNCERTAINTY_MEASURE_WITH_UNIT(LENGTH_MEASURE(1.E-5),#3833,
'DISTANCE_ACCURACY_VALUE',
'Maximum model space distance between geometric entities at asserted c
onnectivities');
#3820=UNCERTAINTY_MEASURE_WITH_UNIT(LENGTH_MEASURE(1.E-5),#3833,
'DISTANCE_ACCURACY_VALUE',
'Maximum model space distance between geometric entities at asserted c
onnectivities');
#3821=UNCERTAINTY_MEASURE_WITH_UNIT(LENGTH_MEASURE(1.E-5),#3833,
'DISTANCE_ACCURACY_VALUE',
'Maximum model space distance between geometric entities at asserted c
onnectivities');
#3822=UNCERTAINTY_MEASURE_WITH_UNIT(LENGTH_MEASURE(1.E-5),#3833,
'DISTANCE_ACCURACY_VALUE',
'Maximum model space distance between geometric entities at asserted c
onnectivities');
#3823=UNCERTAINTY_MEASURE_WITH_UNIT(LENGTH_MEASURE(1.E-5),#3833,
'DISTANCE_ACCURACY_VALUE',
'Maximum model space distance between geometric entities at asserted c
onnectivities');
#3824=UNCERTAINTY_MEASURE_WITH_UNIT(LENGTH_MEASURE(1.E-5),#3833,
'DISTANCE_ACCURACY_VALUE',
'Maximum model space distance between geometric entities at asserted c
onnectivities');
#3825=(
GEOMETRIC_REPRESENTATION_CONTEXT(3)
GLOBAL_UNCERTAINTY_ASSIGNED_CONTEXT((#3817))
GLOBAL_UNIT_ASSIGNED_CONTEXT((#3833,#3834,#3835))
REPRESENTATION_CONTEXT('','3D')
);
#3826=(
GEOMETRIC_REPRESENTATION_CONTEXT(3)
GLOBAL_UNCERTAINTY_ASSIGNED_CONTEXT((#3818))
GLOBAL_UNIT_ASSIGNED_CONTEXT((#3833,#3834,#3835))
REPRESENTATION_CONTEXT('','3D')
);
#3827=(
GEOMETRIC_REPRESENTATION_CONTEXT(3)
GLOBAL_UNCERTAINTY_ASSIGNED_CONTEXT((#3819))
GLOBAL_UNIT_ASSIGNED_CONTEXT((#3833,#3834,#3835))
REPRESENTATION_CONTEXT('','3D')
);
#3828=(
GEOMETRIC_REPRESENTATION_CONTEXT(3)
GLOBAL_UNCERTAINTY_ASSIGNED_CONTEXT((#3820))
GLOBAL_UNIT_ASSIGNED_CONTEXT((#3833,#3834,#3835))
REPRESENTATION_CONTEXT('','3D')
);
#3829=(
GEOMETRIC_REPRESENTATION_CONTEXT(3)
GLOBAL_UNCERTAINTY_ASSIGNED_CONTEXT((#3821))
GLOBAL_UNIT_ASSIGNED_CONTEXT((#3833,#3834,#3835))
REPRESENTATION_CONTEXT('','3D')
);
#3830=(
GEOMETRIC_REPRESENTATION_CONTEXT(3)
GLOBAL_UNCERTAINTY_ASSIGNED_CONTEXT((#3822))
GLOBAL_UNIT_ASSIGNED_CONTEXT((#3833,#3834,#3835))
REPRESENTATION_CONTEXT('','3D')
);
#3831=(
GEOMETRIC_REPRESENTATION_CONTEXT(3)
GLOBAL_UNCERTAINTY_ASSIGNED_CONTEXT((#3823))
GLOBAL_UNIT_ASSIGNED_CONTEXT((#3833,#3834,#3835))
REPRESENTATION_CONTEXT('','3D')
);
#3832=(
GEOMETRIC_REPRESENTATION_CONTEXT(3)
GLOBAL_UNCERTAINTY_ASSIGNED_CONTEXT((#3824))
GLOBAL_UNIT_ASSIGNED_CONTEXT((#3833,#3834,#3835))
REPRESENTATION_CONTEXT('','3D')
);
#3833=(
LENGTH_UNIT()
NAMED_UNIT(*)
SI_UNIT($,.METRE.)
);
#3834=(
NAMED_UNIT(*)
PLANE_ANGLE_UNIT()
SI_UNIT($,.RADIAN.)
);
#3835=(
NAMED_UNIT(*)
SI_UNIT($,.STERADIAN.)
SOLID_ANGLE_UNIT()
);
#3836=SHAPE_DEFINITION_REPRESENTATION(#3843,#3862);
#3837=SHAPE_DEFINITION_REPRESENTATION(#3844,#3863);
#3838=SHAPE_DEFINITION_REPRESENTATION(#3845,#3864);
#3839=SHAPE_DEFINITION_REPRESENTATION(#3846,#3865);
#3840=SHAPE_DEFINITION_REPRESENTATION(#3847,#3866);
#3841=SHAPE_DEFINITION_REPRESENTATION(#3848,#3867);
#3842=SHAPE_DEFINITION_REPRESENTATION(#3849,#3868);
#3843=PRODUCT_DEFINITION_SHAPE('',$,#3870);
#3844=PRODUCT_DEFINITION_SHAPE('',$,#3871);
#3845=PRODUCT_DEFINITION_SHAPE('',$,#3872);
#3846=PRODUCT_DEFINITION_SHAPE('',$,#3873);
#3847=PRODUCT_DEFINITION_SHAPE('',$,#3874);
#3848=PRODUCT_DEFINITION_SHAPE('',$,#3875);
#3849=PRODUCT_DEFINITION_SHAPE('',$,#3876);
#3850=PRODUCT_DEFINITION_SHAPE($,$,#47);
#3851=PRODUCT_DEFINITION_SHAPE($,$,#48);
#3852=PRODUCT_DEFINITION_SHAPE($,$,#49);
#3853=PRODUCT_DEFINITION_SHAPE($,$,#50);
#3854=PRODUCT_DEFINITION_SHAPE($,$,#51);
#3855=PRODUCT_DEFINITION_SHAPE($,$,#52);
#3856=PRODUCT_DEFINITION_SHAPE($,$,#53);
#3857=PRODUCT_DEFINITION_SHAPE($,$,#54);
#3858=PRODUCT_DEFINITION_SHAPE($,$,#55);
#3859=PRODUCT_DEFINITION_SHAPE($,$,#56);
#3860=PRODUCT_DEFINITION_SHAPE($,$,#57);
#3861=PRODUCT_DEFINITION_SHAPE($,$,#58);
#3862=SHAPE_REPRESENTATION('',(#1856,#2036,#2037,#2038,#2039,#2040,#2041,
#2042,#2043,#2044,#2045,#2046,#2047),#3825);
#3863=SHAPE_REPRESENTATION('',(#1857),#3826);
#3864=SHAPE_REPRESENTATION('',(#1874),#3827);
#3865=SHAPE_REPRESENTATION('',(#1880),#3828);
#3866=SHAPE_REPRESENTATION('',(#1915),#3829);
#3867=SHAPE_REPRESENTATION('',(#1951),#3830);
#3868=SHAPE_REPRESENTATION('',(#1986),#3831);
#3869=PRODUCT_DEFINITION_CONTEXT('part definition',#3892,'design');
#3870=PRODUCT_DEFINITION('2026-10-07-08-28-20-685',
'MAS-606',#3877,#3869);
#3871=PRODUCT_DEFINITION('2026-10-07-15-35-32-214','Wheel',#3878,#3869);
#3872=PRODUCT_DEFINITION('2026-10-07-15-36-10-785','Bearings + Bolt',#3879,
#3869);
#3873=PRODUCT_DEFINITION('2026-10-07-15-36-10-347','Wheel_Plate',#3880,
#3869);
#3874=PRODUCT_DEFINITION('2026-10-07-15-36-29-757',
'Hex flange bolt small M6x1.00 x 25',#3881,#3869);
#3875=PRODUCT_DEFINITION('2026-10-07-15-37-59-801',
'Hex flange nut M6x1.00',#3882,#3869);
#3876=PRODUCT_DEFINITION('2026-10-07-08-56-00-255','Wheel_Holder',#3883,
#3869);
#3877=PRODUCT_DEFINITION_FORMATION('',$,#3894);
#3878=PRODUCT_DEFINITION_FORMATION('',$,#3895);
#3879=PRODUCT_DEFINITION_FORMATION('',$,#3896);
#3880=PRODUCT_DEFINITION_FORMATION('',$,#3897);
#3881=PRODUCT_DEFINITION_FORMATION('',$,#3898);
#3882=PRODUCT_DEFINITION_FORMATION('',$,#3899);
#3883=PRODUCT_DEFINITION_FORMATION('',$,#3900);
#3884=PRODUCT_RELATED_PRODUCT_CATEGORY('MAS-606',
'MAS-606',(#3894));
#3885=PRODUCT_RELATED_PRODUCT_CATEGORY('Wheel','Wheel',(#3895));
#3886=PRODUCT_RELATED_PRODUCT_CATEGORY('Bearings + Bolt',
'Bearings + Bolt',(#3896));
#3887=PRODUCT_RELATED_PRODUCT_CATEGORY('Wheel_Plate','Wheel_Plate',(#3897));
#3888=PRODUCT_RELATED_PRODUCT_CATEGORY(
'Hex flange bolt small M6x1.00 x 25',
'Hex flange bolt small M6x1.00 x 25',(#3898));
#3889=PRODUCT_RELATED_PRODUCT_CATEGORY('Hex flange nut M6x1.00',
'Hex flange nut M6x1.00',(#3899));
#3890=PRODUCT_RELATED_PRODUCT_CATEGORY('Wheel_Holder','Wheel_Holder',(#3900));
#3891=APPLICATION_PROTOCOL_DEFINITION('international standard',
'automotive_design',2009,#3892);
#3892=APPLICATION_CONTEXT(
'Core Data for Automotive Mechanical Design Process');
#3893=PRODUCT_CONTEXT('part definition',#3892,'mechanical');
#3894=PRODUCT('2026-10-07-08-28-20-685','MAS-606',
'Wheel Holder-Mirrored',(#3893));
#3895=PRODUCT('2026-10-07-15-35-32-214','Wheel','Wheel',(#3893));
#3896=PRODUCT('2026-10-07-15-36-10-785','Bearings + Bolt',
'Bearings + Bolt',(#3893));
#3897=PRODUCT('2026-10-07-15-36-10-347','Wheel_Plate',
'6mm-4pcs-wheel-plate',(#3893));
#3898=PRODUCT('2026-10-07-15-36-29-757',
'Hex flange bolt small M6x1.00 x 25',
'Hex flange bolt small M6x1.00 x 25',(#3893));
#3899=PRODUCT('2026-10-07-15-37-59-801','Hex flange nut M6x1.00',
'Hex flange nut M6x1.00',(#3893));
#3900=PRODUCT('2026-10-07-08-56-00-255','Wheel_Holder',$,(#3893));
#3901=PRESENTATION_STYLE_ASSIGNMENT((#3907));
#3902=PRESENTATION_STYLE_ASSIGNMENT((#3908));
#3903=PRESENTATION_STYLE_ASSIGNMENT((#3909));
#3904=PRESENTATION_STYLE_ASSIGNMENT((#3910));
#3905=PRESENTATION_STYLE_ASSIGNMENT((#3911));
#3906=PRESENTATION_STYLE_ASSIGNMENT((#3912));
#3907=SURFACE_STYLE_USAGE(.BOTH.,#3913);
#3908=SURFACE_STYLE_USAGE(.BOTH.,#3914);
#3909=SURFACE_STYLE_USAGE(.BOTH.,#3915);
#3910=SURFACE_STYLE_USAGE(.BOTH.,#3916);
#3911=SURFACE_STYLE_USAGE(.BOTH.,#3917);
#3912=SURFACE_STYLE_USAGE(.BOTH.,#3918);
#3913=SURFACE_SIDE_STYLE('',(#3919));
#3914=SURFACE_SIDE_STYLE('',(#3920));
#3915=SURFACE_SIDE_STYLE('',(#3921));
#3916=SURFACE_SIDE_STYLE('',(#3922));
#3917=SURFACE_SIDE_STYLE('',(#3923));
#3918=SURFACE_SIDE_STYLE('',(#3924));
#3919=SURFACE_STYLE_FILL_AREA(#3925);
#3920=SURFACE_STYLE_FILL_AREA(#3926);
#3921=SURFACE_STYLE_FILL_AREA(#3927);
#3922=SURFACE_STYLE_FILL_AREA(#3928);
#3923=SURFACE_STYLE_FILL_AREA(#3929);
#3924=SURFACE_STYLE_FILL_AREA(#3930);
#3925=FILL_AREA_STYLE('Steel - Satin',(#3931));
#3926=FILL_AREA_STYLE('Opaque(59,97,180)',(#3932));
#3927=FILL_AREA_STYLE('Opaque(234,234,234)',(#3933));
#3928=FILL_AREA_STYLE('Opaque(157,207,237)',(#3934));
#3929=FILL_AREA_STYLE('Opaque(154,165,175)',(#3935));
#3930=FILL_AREA_STYLE('Opaque(248,135,1)',(#3936));
#3931=FILL_AREA_STYLE_COLOUR('Steel - Satin',#3937);
#3932=FILL_AREA_STYLE_COLOUR('Opaque(59,97,180)',#3938);
#3933=FILL_AREA_STYLE_COLOUR('Opaque(234,234,234)',#3939);
#3934=FILL_AREA_STYLE_COLOUR('Opaque(157,207,237)',#3940);
#3935=FILL_AREA_STYLE_COLOUR('Opaque(154,165,175)',#3941);
#3936=FILL_AREA_STYLE_COLOUR('Opaque(248,135,1)',#3942);
#3937=COLOUR_RGB('Steel - Satin', 0.09019608, 0.27058824, 0.51372549);
#3938=COLOUR_RGB('Opaque(59,97,180)', 0.09019608, 0.27058824, 0.51372549);
#3939=COLOUR_RGB('Opaque(234,234,234)', 0.66274510, 0.83137255, 0.94901961);
#3940=COLOUR_RGB('Opaque(157,207,237)', 0.31764706, 0.68627451, 0.89019608);
#3941=COLOUR_RGB('Opaque(154,165,175)', 0.40784314, 0.44705882, 0.49803922);
#3942=COLOUR_RGB('Opaque(248,135,1)', 0.08235294, 0.09019608, 0.10196078);
ENDSEC;
END-ISO-10303-21;
